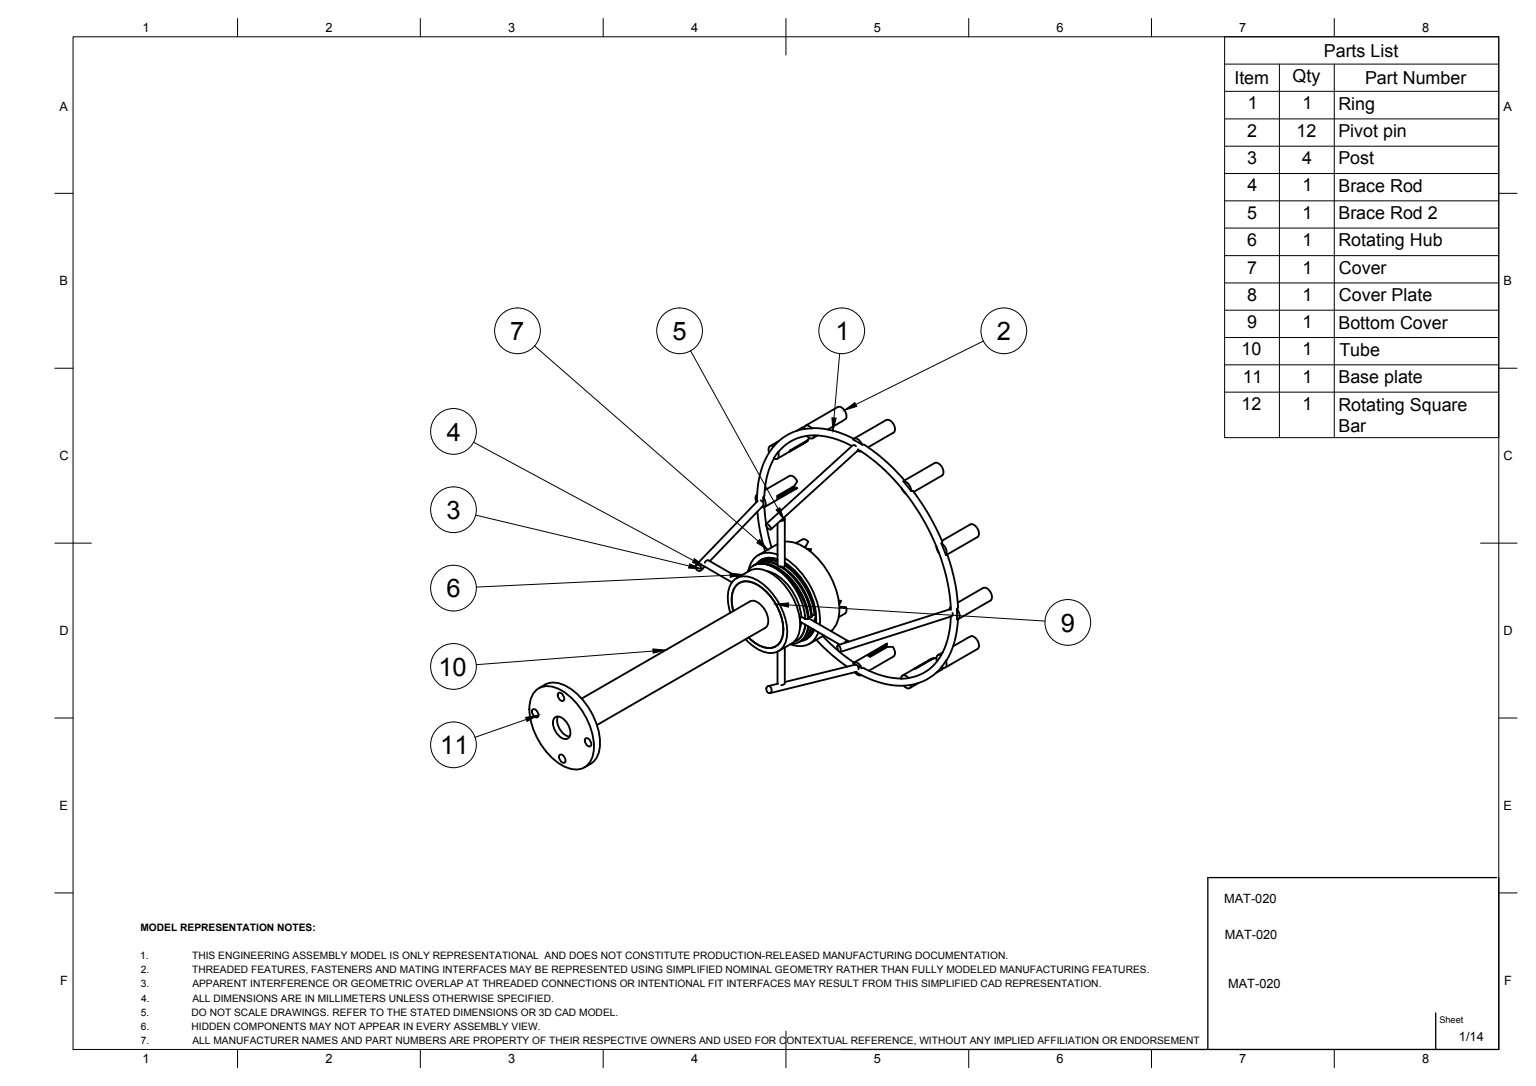
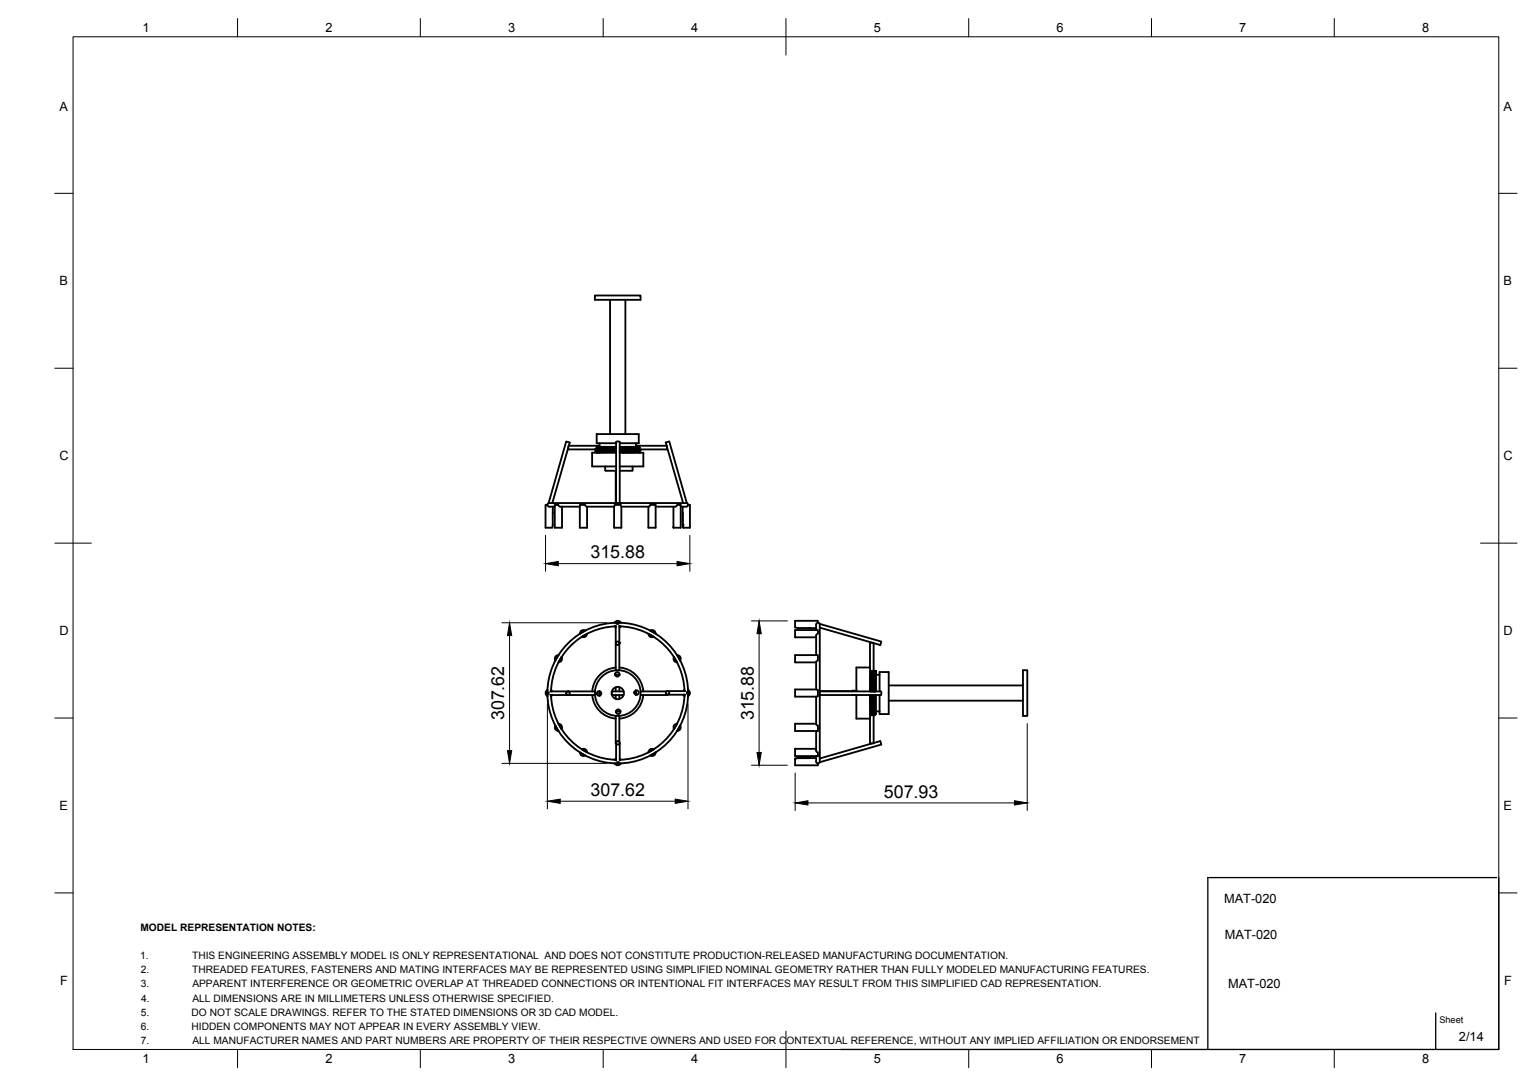
ISO-10303-21;
HEADER;
/* Generated by software containing ST-Developer
 * from STEP Tools, Inc. (www.steptools.com) 
 */

FILE_DESCRIPTION(
/* description */ ('STEP AP214'),
/* implementation_level */ '2;1');

FILE_NAME(
/* name */ 'MAT-020.step',
/* time_stamp */ '2026-11-14T06:20:50-08:00',
/* author */ (''),
/* organization */ (''),
/* preprocessor_version */ 'ST-DEVELOPER v20.2',
/* originating_system */ 'Autodesk Translation Framework v15.17.0.0',
/* authorisation */ '');

FILE_SCHEMA (('AUTOMOTIVE_DESIGN { 1 0 10303 214 3 1 1 }'));
ENDSEC;

DATA;
#10=MECHANICAL_DESIGN_GEOMETRIC_PRESENTATION_REPRESENTATION('',(#956,#957,
#958,#959,#960,#961,#962,#963,#964,#965,#966,#967),#20658);
#11=ITEM_DEFINED_TRANSFORMATION($,$,#3797,#4103);
#12=ITEM_DEFINED_TRANSFORMATION($,$,#4072,#4104);
#13=ITEM_DEFINED_TRANSFORMATION($,$,#4066,#4105);
#14=ITEM_DEFINED_TRANSFORMATION($,$,#3801,#4106);
#15=ITEM_DEFINED_TRANSFORMATION($,$,#3807,#4107);
#16=ITEM_DEFINED_TRANSFORMATION($,$,#3813,#4108);
#17=ITEM_DEFINED_TRANSFORMATION($,$,#3932,#4109);
#18=ITEM_DEFINED_TRANSFORMATION($,$,#3966,#4110);
#19=ITEM_DEFINED_TRANSFORMATION($,$,#3972,#4111);
#20=ITEM_DEFINED_TRANSFORMATION($,$,#3981,#4112);
#21=ITEM_DEFINED_TRANSFORMATION($,$,#3990,#4113);
#22=ITEM_DEFINED_TRANSFORMATION($,$,#4015,#4114);
#23=ITEM_DEFINED_TRANSFORMATION($,$,#4066,#4115);
#24=ITEM_DEFINED_TRANSFORMATION($,$,#4066,#4116);
#25=ITEM_DEFINED_TRANSFORMATION($,$,#4066,#4117);
#26=ITEM_DEFINED_TRANSFORMATION($,$,#4072,#4118);
#27=ITEM_DEFINED_TRANSFORMATION($,$,#4072,#4119);
#28=ITEM_DEFINED_TRANSFORMATION($,$,#4072,#4120);
#29=ITEM_DEFINED_TRANSFORMATION($,$,#4072,#4121);
#30=ITEM_DEFINED_TRANSFORMATION($,$,#4072,#4122);
#31=ITEM_DEFINED_TRANSFORMATION($,$,#4072,#4123);
#32=ITEM_DEFINED_TRANSFORMATION($,$,#4072,#4124);
#33=ITEM_DEFINED_TRANSFORMATION($,$,#4072,#4125);
#34=ITEM_DEFINED_TRANSFORMATION($,$,#4072,#4126);
#35=ITEM_DEFINED_TRANSFORMATION($,$,#4072,#4127);
#36=ITEM_DEFINED_TRANSFORMATION($,$,#4072,#4128);
#37=(
REPRESENTATION_RELATIONSHIP($,$,#20716,#20715)
REPRESENTATION_RELATIONSHIP_WITH_TRANSFORMATION(#11)
SHAPE_REPRESENTATION_RELATIONSHIP()
);
#38=(
REPRESENTATION_RELATIONSHIP($,$,#20727,#20715)
REPRESENTATION_RELATIONSHIP_WITH_TRANSFORMATION(#12)
SHAPE_REPRESENTATION_RELATIONSHIP()
);
#39=(
REPRESENTATION_RELATIONSHIP($,$,#20726,#20715)
REPRESENTATION_RELATIONSHIP_WITH_TRANSFORMATION(#13)
SHAPE_REPRESENTATION_RELATIONSHIP()
);
#40=(
REPRESENTATION_RELATIONSHIP($,$,#20717,#20715)
REPRESENTATION_RELATIONSHIP_WITH_TRANSFORMATION(#14)
SHAPE_REPRESENTATION_RELATIONSHIP()
);
#41=(
REPRESENTATION_RELATIONSHIP($,$,#20718,#20715)
REPRESENTATION_RELATIONSHIP_WITH_TRANSFORMATION(#15)
SHAPE_REPRESENTATION_RELATIONSHIP()
);
#42=(
REPRESENTATION_RELATIONSHIP($,$,#20719,#20715)
REPRESENTATION_RELATIONSHIP_WITH_TRANSFORMATION(#16)
SHAPE_REPRESENTATION_RELATIONSHIP()
);
#43=(
REPRESENTATION_RELATIONSHIP($,$,#20720,#20715)
REPRESENTATION_RELATIONSHIP_WITH_TRANSFORMATION(#17)
SHAPE_REPRESENTATION_RELATIONSHIP()
);
#44=(
REPRESENTATION_RELATIONSHIP($,$,#20721,#20715)
REPRESENTATION_RELATIONSHIP_WITH_TRANSFORMATION(#18)
SHAPE_REPRESENTATION_RELATIONSHIP()
);
#45=(
REPRESENTATION_RELATIONSHIP($,$,#20722,#20715)
REPRESENTATION_RELATIONSHIP_WITH_TRANSFORMATION(#19)
SHAPE_REPRESENTATION_RELATIONSHIP()
);
#46=(
REPRESENTATION_RELATIONSHIP($,$,#20723,#20715)
REPRESENTATION_RELATIONSHIP_WITH_TRANSFORMATION(#20)
SHAPE_REPRESENTATION_RELATIONSHIP()
);
#47=(
REPRESENTATION_RELATIONSHIP($,$,#20724,#20715)
REPRESENTATION_RELATIONSHIP_WITH_TRANSFORMATION(#21)
SHAPE_REPRESENTATION_RELATIONSHIP()
);
#48=(
REPRESENTATION_RELATIONSHIP($,$,#20725,#20715)
REPRESENTATION_RELATIONSHIP_WITH_TRANSFORMATION(#22)
SHAPE_REPRESENTATION_RELATIONSHIP()
);
#49=(
REPRESENTATION_RELATIONSHIP($,$,#20726,#20715)
REPRESENTATION_RELATIONSHIP_WITH_TRANSFORMATION(#23)
SHAPE_REPRESENTATION_RELATIONSHIP()
);
#50=(
REPRESENTATION_RELATIONSHIP($,$,#20726,#20715)
REPRESENTATION_RELATIONSHIP_WITH_TRANSFORMATION(#24)
SHAPE_REPRESENTATION_RELATIONSHIP()
);
#51=(
REPRESENTATION_RELATIONSHIP($,$,#20726,#20715)
REPRESENTATION_RELATIONSHIP_WITH_TRANSFORMATION(#25)
SHAPE_REPRESENTATION_RELATIONSHIP()
);
#52=(
REPRESENTATION_RELATIONSHIP($,$,#20727,#20715)
REPRESENTATION_RELATIONSHIP_WITH_TRANSFORMATION(#26)
SHAPE_REPRESENTATION_RELATIONSHIP()
);
#53=(
REPRESENTATION_RELATIONSHIP($,$,#20727,#20715)
REPRESENTATION_RELATIONSHIP_WITH_TRANSFORMATION(#27)
SHAPE_REPRESENTATION_RELATIONSHIP()
);
#54=(
REPRESENTATION_RELATIONSHIP($,$,#20727,#20715)
REPRESENTATION_RELATIONSHIP_WITH_TRANSFORMATION(#28)
SHAPE_REPRESENTATION_RELATIONSHIP()
);
#55=(
REPRESENTATION_RELATIONSHIP($,$,#20727,#20715)
REPRESENTATION_RELATIONSHIP_WITH_TRANSFORMATION(#29)
SHAPE_REPRESENTATION_RELATIONSHIP()
);
#56=(
REPRESENTATION_RELATIONSHIP($,$,#20727,#20715)
REPRESENTATION_RELATIONSHIP_WITH_TRANSFORMATION(#30)
SHAPE_REPRESENTATION_RELATIONSHIP()
);
#57=(
REPRESENTATION_RELATIONSHIP($,$,#20727,#20715)
REPRESENTATION_RELATIONSHIP_WITH_TRANSFORMATION(#31)
SHAPE_REPRESENTATION_RELATIONSHIP()
);
#58=(
REPRESENTATION_RELATIONSHIP($,$,#20727,#20715)
REPRESENTATION_RELATIONSHIP_WITH_TRANSFORMATION(#32)
SHAPE_REPRESENTATION_RELATIONSHIP()
);
#59=(
REPRESENTATION_RELATIONSHIP($,$,#20727,#20715)
REPRESENTATION_RELATIONSHIP_WITH_TRANSFORMATION(#33)
SHAPE_REPRESENTATION_RELATIONSHIP()
);
#60=(
REPRESENTATION_RELATIONSHIP($,$,#20727,#20715)
REPRESENTATION_RELATIONSHIP_WITH_TRANSFORMATION(#34)
SHAPE_REPRESENTATION_RELATIONSHIP()
);
#61=(
REPRESENTATION_RELATIONSHIP($,$,#20727,#20715)
REPRESENTATION_RELATIONSHIP_WITH_TRANSFORMATION(#35)
SHAPE_REPRESENTATION_RELATIONSHIP()
);
#62=(
REPRESENTATION_RELATIONSHIP($,$,#20727,#20715)
REPRESENTATION_RELATIONSHIP_WITH_TRANSFORMATION(#36)
SHAPE_REPRESENTATION_RELATIONSHIP()
);
#63=CONTEXT_DEPENDENT_SHAPE_REPRESENTATION(#37,#20689);
#64=CONTEXT_DEPENDENT_SHAPE_REPRESENTATION(#38,#20690);
#65=CONTEXT_DEPENDENT_SHAPE_REPRESENTATION(#39,#20691);
#66=CONTEXT_DEPENDENT_SHAPE_REPRESENTATION(#40,#20692);
#67=CONTEXT_DEPENDENT_SHAPE_REPRESENTATION(#41,#20693);
#68=CONTEXT_DEPENDENT_SHAPE_REPRESENTATION(#42,#20694);
#69=CONTEXT_DEPENDENT_SHAPE_REPRESENTATION(#43,#20695);
#70=CONTEXT_DEPENDENT_SHAPE_REPRESENTATION(#44,#20696);
#71=CONTEXT_DEPENDENT_SHAPE_REPRESENTATION(#45,#20697);
#72=CONTEXT_DEPENDENT_SHAPE_REPRESENTATION(#46,#20698);
#73=CONTEXT_DEPENDENT_SHAPE_REPRESENTATION(#47,#20699);
#74=CONTEXT_DEPENDENT_SHAPE_REPRESENTATION(#48,#20700);
#75=CONTEXT_DEPENDENT_SHAPE_REPRESENTATION(#49,#20701);
#76=CONTEXT_DEPENDENT_SHAPE_REPRESENTATION(#50,#20702);
#77=CONTEXT_DEPENDENT_SHAPE_REPRESENTATION(#51,#20703);
#78=CONTEXT_DEPENDENT_SHAPE_REPRESENTATION(#52,#20704);
#79=CONTEXT_DEPENDENT_SHAPE_REPRESENTATION(#53,#20705);
#80=CONTEXT_DEPENDENT_SHAPE_REPRESENTATION(#54,#20706);
#81=CONTEXT_DEPENDENT_SHAPE_REPRESENTATION(#55,#20707);
#82=CONTEXT_DEPENDENT_SHAPE_REPRESENTATION(#56,#20708);
#83=CONTEXT_DEPENDENT_SHAPE_REPRESENTATION(#57,#20709);
#84=CONTEXT_DEPENDENT_SHAPE_REPRESENTATION(#58,#20710);
#85=CONTEXT_DEPENDENT_SHAPE_REPRESENTATION(#59,#20711);
#86=CONTEXT_DEPENDENT_SHAPE_REPRESENTATION(#60,#20712);
#87=CONTEXT_DEPENDENT_SHAPE_REPRESENTATION(#61,#20713);
#88=CONTEXT_DEPENDENT_SHAPE_REPRESENTATION(#62,#20714);
#89=NEXT_ASSEMBLY_USAGE_OCCURRENCE('Ring:1','Ring:1','Ring:1',#20729,#20730,
'Ring:1');
#90=NEXT_ASSEMBLY_USAGE_OCCURRENCE('Pivot Pin:1','Pivot Pin:1',
'Pivot Pin:1',#20729,#20741,'Pivot Pin:1');
#91=NEXT_ASSEMBLY_USAGE_OCCURRENCE('Post:1','Post:1','Post:1',#20729,#20740,
'Post:1');
#92=NEXT_ASSEMBLY_USAGE_OCCURRENCE('Brace Rod:1','Brace Rod:1',
'Brace Rod:1',#20729,#20731,'Brace Rod:1');
#93=NEXT_ASSEMBLY_USAGE_OCCURRENCE('Brace Rod 2:1','Brace Rod 2:1',
'Brace Rod 2:1',#20729,#20732,'Brace Rod 2:1');
#94=NEXT_ASSEMBLY_USAGE_OCCURRENCE('Rotating Hub:1','Rotating Hub:1',
'Rotating Hub:1',#20729,#20733,'Rotating Hub:1');
#95=NEXT_ASSEMBLY_USAGE_OCCURRENCE('Cover:1','Cover:1','Cover:1',#20729,
#20734,'Cover:1');
#96=NEXT_ASSEMBLY_USAGE_OCCURRENCE('Cover Plate:1','Cover Plate:1',
'Cover Plate:1',#20729,#20735,'Cover Plate:1');
#97=NEXT_ASSEMBLY_USAGE_OCCURRENCE('Bottom Cover:1','Bottom Cover:1',
'Bottom Cover:1',#20729,#20736,'Bottom Cover:1');
#98=NEXT_ASSEMBLY_USAGE_OCCURRENCE('Tube:1','Tube:1','Tube:1',#20729,#20737,
'Tube:1');
#99=NEXT_ASSEMBLY_USAGE_OCCURRENCE('Base Plate:1','Base Plate:1',
'Base Plate:1',#20729,#20738,'Base Plate:1');
#100=NEXT_ASSEMBLY_USAGE_OCCURRENCE('Rotating Square Bar:1',
'Rotating Square Bar:1','Rotating Square Bar:1',#20729,#20739,
'Rotating Square Bar:1');
#101=NEXT_ASSEMBLY_USAGE_OCCURRENCE('Post:2','Post:2','Post:2',#20729,#20740,
'Post:2');
#102=NEXT_ASSEMBLY_USAGE_OCCURRENCE('Post:3','Post:3','Post:3',#20729,#20740,
'Post:3');
#103=NEXT_ASSEMBLY_USAGE_OCCURRENCE('Post:4','Post:4','Post:4',#20729,#20740,
'Post:4');
#104=NEXT_ASSEMBLY_USAGE_OCCURRENCE('Pivot Pin:2','Pivot Pin:2',
'Pivot Pin:2',#20729,#20741,'Pivot Pin:2');
#105=NEXT_ASSEMBLY_USAGE_OCCURRENCE('Pivot Pin:3','Pivot Pin:3',
'Pivot Pin:3',#20729,#20741,'Pivot Pin:3');
#106=NEXT_ASSEMBLY_USAGE_OCCURRENCE('Pivot Pin:4','Pivot Pin:4',
'Pivot Pin:4',#20729,#20741,'Pivot Pin:4');
#107=NEXT_ASSEMBLY_USAGE_OCCURRENCE('Pivot Pin:5','Pivot Pin:5',
'Pivot Pin:5',#20729,#20741,'Pivot Pin:5');
#108=NEXT_ASSEMBLY_USAGE_OCCURRENCE('Pivot Pin:6','Pivot Pin:6',
'Pivot Pin:6',#20729,#20741,'Pivot Pin:6');
#109=NEXT_ASSEMBLY_USAGE_OCCURRENCE('Pivot Pin:7','Pivot Pin:7',
'Pivot Pin:7',#20729,#20741,'Pivot Pin:7');
#110=NEXT_ASSEMBLY_USAGE_OCCURRENCE('Pivot Pin:8','Pivot Pin:8',
'Pivot Pin:8',#20729,#20741,'Pivot Pin:8');
#111=NEXT_ASSEMBLY_USAGE_OCCURRENCE('Pivot Pin:9','Pivot Pin:9',
'Pivot Pin:9',#20729,#20741,'Pivot Pin:9');
#112=NEXT_ASSEMBLY_USAGE_OCCURRENCE('Pivot Pin:10','Pivot Pin:10',
'Pivot Pin:10',#20729,#20741,'Pivot Pin:10');
#113=NEXT_ASSEMBLY_USAGE_OCCURRENCE('Pivot Pin:11','Pivot Pin:11',
'Pivot Pin:11',#20729,#20741,'Pivot Pin:11');
#114=NEXT_ASSEMBLY_USAGE_OCCURRENCE('Pivot Pin:12','Pivot Pin:12',
'Pivot Pin:12',#20729,#20741,'Pivot Pin:12');
#115=CONICAL_SURFACE('',#4073,6.35000000000001,0.785398163397456);
#116=SPHERICAL_SURFACE('',#4025,1.);
#117=SPHERICAL_SURFACE('',#4028,1.);
#118=SPHERICAL_SURFACE('',#4045,1.);
#119=SPHERICAL_SURFACE('',#4047,1.);
#120=SPHERICAL_SURFACE('',#4049,1.);
#121=SPHERICAL_SURFACE('',#4051,1.);
#122=SPHERICAL_SURFACE('',#4061,1.);
#123=SPHERICAL_SURFACE('',#4063,1.);
#124=FACE_BOUND('',#1300,.T.);
#125=FACE_BOUND('',#1302,.T.);
#126=FACE_BOUND('',#1314,.T.);
#127=FACE_BOUND('',#1332,.T.);
#128=FACE_BOUND('',#1334,.T.);
#129=FACE_BOUND('',#1338,.T.);
#130=FACE_BOUND('',#1340,.T.);
#131=FACE_BOUND('',#1342,.T.);
#132=FACE_BOUND('',#1349,.T.);
#133=FACE_BOUND('',#1351,.T.);
#134=FACE_BOUND('',#1355,.T.);
#135=FACE_BOUND('',#1357,.T.);
#136=FACE_BOUND('',#1366,.T.);
#137=FACE_BOUND('',#1367,.T.);
#138=FACE_BOUND('',#1368,.T.);
#139=FACE_BOUND('',#1369,.T.);
#140=FACE_BOUND('',#1370,.T.);
#141=FACE_BOUND('',#1372,.T.);
#142=FACE_BOUND('',#1373,.T.);
#143=FACE_BOUND('',#1374,.T.);
#144=FACE_BOUND('',#1375,.T.);
#145=FACE_BOUND('',#1376,.T.);
#146=FACE_BOUND('',#1378,.T.);
#147=ELLIPSE('',#3911,3.97203818895926,3.95968922073708);
#148=ELLIPSE('',#4079,13.8289418104825,6.34999999998296);
#149=ELLIPSE('',#4080,15.0727020037017,6.35000000001005);
#150=ELLIPSE('',#4086,17.286177263089,7.93749999997138);
#151=ELLIPSE('',#4088,18.840877504683,7.93750000004892);
#152=(
BOUNDED_SURFACE()
B_SPLINE_SURFACE(1,2,((#5540,#5541,#5542,#5543,#5544,#5545,#5546,#5547,
#5548,#5549,#5550,#5551,#5552,#5553,#5554,#5555,#5556,#5557,#5558,#5559,
#5560,#5561,#5562,#5563,#5564,#5565,#5566,#5567,#5568,#5569,#5570,#5571,
#5572,#5573,#5574,#5575,#5576,#5577,#5578,#5579,#5580,#5581,#5582,#5583,
#5584,#5585,#5586,#5587,#5588,#5589,#5590,#5591,#5592,#5593,#5594,#5595,
#5596,#5597,#5598,#5599,#5600,#5601,#5602,#5603,#5604,#5605,#5606,#5607,
#5608,#5609,#5610,#5611,#5612,#5613,#5614,#5615,#5616,#5617,#5618,#5619,
#5620,#5621,#5622,#5623,#5624,#5625,#5626,#5627,#5628,#5629,#5630,#5631,
#5632,#5633,#5634,#5635,#5636,#5637,#5638,#5639,#5640,#5641,#5642,#5643,
#5644,#5645,#5646,#5647,#5648,#5649,#5650,#5651,#5652,#5653,#5654,#5655,
#5656,#5657,#5658,#5659,#5660,#5661,#5662,#5663,#5664,#5665,#5666,#5667,
#5668,#5669,#5670,#5671,#5672,#5673,#5674,#5675,#5676,#5677,#5678,#5679,
#5680,#5681,#5682,#5683,#5684),(#5685,#5686,#5687,#5688,#5689,#5690,#5691,
#5692,#5693,#5694,#5695,#5696,#5697,#5698,#5699,#5700,#5701,#5702,#5703,
#5704,#5705,#5706,#5707,#5708,#5709,#5710,#5711,#5712,#5713,#5714,#5715,
#5716,#5717,#5718,#5719,#5720,#5721,#5722,#5723,#5724,#5725,#5726,#5727,
#5728,#5729,#5730,#5731,#5732,#5733,#5734,#5735,#5736,#5737,#5738,#5739,
#5740,#5741,#5742,#5743,#5744,#5745,#5746,#5747,#5748,#5749,#5750,#5751,
#5752,#5753,#5754,#5755,#5756,#5757,#5758,#5759,#5760,#5761,#5762,#5763,
#5764,#5765,#5766,#5767,#5768,#5769,#5770,#5771,#5772,#5773,#5774,#5775,
#5776,#5777,#5778,#5779,#5780,#5781,#5782,#5783,#5784,#5785,#5786,#5787,
#5788,#5789,#5790,#5791,#5792,#5793,#5794,#5795,#5796,#5797,#5798,#5799,
#5800,#5801,#5802,#5803,#5804,#5805,#5806,#5807,#5808,#5809,#5810,#5811,
#5812,#5813,#5814,#5815,#5816,#5817,#5818,#5819,#5820,#5821,#5822,#5823,
#5824,#5825,#5826,#5827,#5828,#5829)),.UNSPECIFIED.,.F.,.F.,.F.)
B_SPLINE_SURFACE_WITH_KNOTS((2,2),(3,2,2,2,2,2,2,2,2,2,2,2,2,2,2,2,2,2,
2,2,2,2,2,2,2,2,2,2,2,2,2,2,2,2,2,2,2,2,2,2,2,2,2,2,2,2,2,2,2,2,2,2,2,2,
2,2,2,2,2,2,2,2,2,2,2,2,2,2,2,2,2,2,3),(0.,1.),(0.,0.0138888888888889,0.0277777777777778,
0.0416666666666667,0.0555555555555556,0.0694444444444444,0.0833333333333333,
0.0972222222222222,0.111111111111111,0.125,0.138888888888889,0.152777777777778,
0.166666666666667,0.180555555555556,0.194444444444444,0.208333333333333,
0.222222222222222,0.236111111111111,0.25,0.263888888888889,0.277777777777778,
0.291666666666667,0.305555555555556,0.319444444444444,0.333333333333333,
0.347222222222222,0.361111111111111,0.375,0.388888888888889,0.402777777777778,
0.416666666666667,0.430555555555556,0.444444444444444,0.458333333333333,
0.472222222222222,0.486111111111111,0.5,0.513888888888889,0.527777777777778,
0.541666666666667,0.555555555555556,0.569444444444444,0.583333333333333,
0.597222222222222,0.611111111111111,0.625,0.638888888888889,0.652777777777778,
0.666666666666667,0.680555555555556,0.694444444444444,0.708333333333333,
0.722222222222222,0.736111111111111,0.75,0.763888888888889,0.777777777777778,
0.791666666666667,0.805555555555556,0.819444444444444,0.833333333333333,
0.847222222222222,0.861111111111111,0.875,0.888888888888889,0.902777777777778,
0.916666666666667,0.930555555555556,0.944444444444444,0.958333333333333,
0.972222222222222,0.986111111111111,1.),.UNSPECIFIED.)
GEOMETRIC_REPRESENTATION_ITEM()
RATIONAL_B_SPLINE_SURFACE(((1.,0.965925826289068,1.,0.965925826289068,1.,
0.965925826289068,1.,0.965925826289068,1.,0.965925826289068,1.,0.965925826289068,
1.,0.965925826289068,1.,0.965925826289068,1.,0.965925826289068,1.,0.965925826289068,
1.,0.965925826289068,1.,0.965925826289068,1.,0.965925826289068,1.,0.965925826289068,
1.,0.965925826289068,1.,0.965925826289068,1.,0.965925826289068,1.,0.965925826289068,
1.,0.965925826289068,1.,0.965925826289068,1.,0.965925826289068,1.,0.965925826289068,
1.,0.965925826289068,1.,0.965925826289068,1.,0.965925826289068,1.,0.965925826289068,
1.,0.965925826289068,1.,0.965925826289068,1.,0.965925826289068,1.,0.965925826289068,
1.,0.965925826289068,1.,0.965925826289068,1.,0.965925826289068,1.,0.965925826289068,
1.,0.965925826289068,1.,0.965925826289068,1.,0.965925826289068,1.,0.965925826289068,
1.,0.965925826289068,1.,0.965925826289068,1.,0.965925826289068,1.,0.965925826289068,
1.,0.965925826289068,1.,0.965925826289068,1.,0.965925826289068,1.,0.965925826289068,
1.,0.965925826289068,1.,0.965925826289068,1.,0.965925826289068,1.,0.965925826289068,
1.,0.965925826289068,1.,0.965925826289068,1.,0.965925826289068,1.,0.965925826289068,
1.,0.965925826289068,1.,0.965925826289068,1.,0.965925826289068,1.,0.965925826289068,
1.,0.965925826289068,1.,0.965925826289068,1.,0.965925826289068,1.,0.965925826289068,
1.,0.965925826289068,1.,0.965925826289068,1.,0.965925826289068,1.,0.965925826289068,
1.,0.965925826289068,1.,0.965925826289068,1.,0.965925826289068,1.,0.965925826289068,
1.,0.965925826289068,1.,0.965925826289068,1.),(1.,0.965925826289068,1.,
0.965925826289068,1.,0.965925826289068,1.,0.965925826289068,1.,0.965925826289068,
1.,0.965925826289068,1.,0.965925826289068,1.,0.965925826289068,1.,0.965925826289068,
1.,0.965925826289068,1.,0.965925826289068,1.,0.965925826289068,1.,0.965925826289068,
1.,0.965925826289068,1.,0.965925826289068,1.,0.965925826289068,1.,0.965925826289068,
1.,0.965925826289068,1.,0.965925826289068,1.,0.965925826289068,1.,0.965925826289068,
1.,0.965925826289068,1.,0.965925826289068,1.,0.965925826289068,1.,0.965925826289068,
1.,0.965925826289068,1.,0.965925826289068,1.,0.965925826289068,1.,0.965925826289068,
1.,0.965925826289068,1.,0.965925826289068,1.,0.965925826289068,1.,0.965925826289068,
1.,0.965925826289068,1.,0.965925826289068,1.,0.965925826289068,1.,0.965925826289068,
1.,0.965925826289068,1.,0.965925826289068,1.,0.965925826289068,1.,0.965925826289068,
1.,0.965925826289068,1.,0.965925826289068,1.,0.965925826289068,1.,0.965925826289068,
1.,0.965925826289068,1.,0.965925826289068,1.,0.965925826289068,1.,0.965925826289068,
1.,0.965925826289068,1.,0.965925826289068,1.,0.965925826289068,1.,0.965925826289068,
1.,0.965925826289068,1.,0.965925826289068,1.,0.965925826289068,1.,0.965925826289068,
1.,0.965925826289068,1.,0.965925826289068,1.,0.965925826289068,1.,0.965925826289068,
1.,0.965925826289068,1.,0.965925826289068,1.,0.965925826289068,1.,0.965925826289068,
1.,0.965925826289068,1.,0.965925826289068,1.,0.965925826289068,1.,0.965925826289068,
1.,0.965925826289068,1.,0.965925826289068,1.,0.965925826289068,1.)))
REPRESENTATION_ITEM('')
SURFACE()
);
#153=(
BOUNDED_SURFACE()
B_SPLINE_SURFACE(1,2,((#5847,#5848,#5849,#5850,#5851,#5852,#5853,#5854,
#5855,#5856,#5857,#5858,#5859,#5860,#5861,#5862,#5863,#5864,#5865,#5866,
#5867,#5868,#5869,#5870,#5871,#5872,#5873,#5874,#5875,#5876,#5877,#5878,
#5879,#5880,#5881,#5882,#5883,#5884,#5885,#5886,#5887,#5888,#5889,#5890,
#5891,#5892,#5893,#5894,#5895,#5896,#5897,#5898,#5899,#5900,#5901,#5902,
#5903,#5904,#5905,#5906,#5907,#5908,#5909,#5910,#5911,#5912,#5913,#5914,
#5915,#5916,#5917,#5918,#5919,#5920,#5921,#5922,#5923,#5924,#5925,#5926,
#5927,#5928,#5929,#5930,#5931,#5932,#5933,#5934,#5935,#5936,#5937,#5938,
#5939,#5940,#5941,#5942,#5943,#5944,#5945,#5946,#5947,#5948,#5949,#5950,
#5951,#5952,#5953,#5954,#5955,#5956,#5957,#5958,#5959,#5960,#5961,#5962,
#5963,#5964,#5965,#5966,#5967,#5968,#5969,#5970,#5971,#5972,#5973,#5974,
#5975,#5976,#5977,#5978,#5979,#5980,#5981,#5982,#5983,#5984,#5985,#5986,
#5987,#5988,#5989,#5990,#5991),(#5992,#5993,#5994,#5995,#5996,#5997,#5998,
#5999,#6000,#6001,#6002,#6003,#6004,#6005,#6006,#6007,#6008,#6009,#6010,
#6011,#6012,#6013,#6014,#6015,#6016,#6017,#6018,#6019,#6020,#6021,#6022,
#6023,#6024,#6025,#6026,#6027,#6028,#6029,#6030,#6031,#6032,#6033,#6034,
#6035,#6036,#6037,#6038,#6039,#6040,#6041,#6042,#6043,#6044,#6045,#6046,
#6047,#6048,#6049,#6050,#6051,#6052,#6053,#6054,#6055,#6056,#6057,#6058,
#6059,#6060,#6061,#6062,#6063,#6064,#6065,#6066,#6067,#6068,#6069,#6070,
#6071,#6072,#6073,#6074,#6075,#6076,#6077,#6078,#6079,#6080,#6081,#6082,
#6083,#6084,#6085,#6086,#6087,#6088,#6089,#6090,#6091,#6092,#6093,#6094,
#6095,#6096,#6097,#6098,#6099,#6100,#6101,#6102,#6103,#6104,#6105,#6106,
#6107,#6108,#6109,#6110,#6111,#6112,#6113,#6114,#6115,#6116,#6117,#6118,
#6119,#6120,#6121,#6122,#6123,#6124,#6125,#6126,#6127,#6128,#6129,#6130,
#6131,#6132,#6133,#6134,#6135,#6136)),.UNSPECIFIED.,.F.,.F.,.F.)
B_SPLINE_SURFACE_WITH_KNOTS((2,2),(3,2,2,2,2,2,2,2,2,2,2,2,2,2,2,2,2,2,
2,2,2,2,2,2,2,2,2,2,2,2,2,2,2,2,2,2,2,2,2,2,2,2,2,2,2,2,2,2,2,2,2,2,2,2,
2,2,2,2,2,2,2,2,2,2,2,2,2,2,2,2,2,2,3),(0.,1.),(0.,0.0138888888888889,0.0277777777777778,
0.0416666666666667,0.0555555555555556,0.0694444444444444,0.0833333333333333,
0.0972222222222222,0.111111111111111,0.125,0.138888888888889,0.152777777777778,
0.166666666666667,0.180555555555556,0.194444444444444,0.208333333333333,
0.222222222222222,0.236111111111111,0.25,0.263888888888889,0.277777777777778,
0.291666666666667,0.305555555555556,0.319444444444444,0.333333333333333,
0.347222222222222,0.361111111111111,0.375,0.388888888888889,0.402777777777778,
0.416666666666667,0.430555555555556,0.444444444444444,0.458333333333333,
0.472222222222222,0.486111111111111,0.5,0.513888888888889,0.527777777777778,
0.541666666666667,0.555555555555556,0.569444444444444,0.583333333333333,
0.597222222222222,0.611111111111111,0.625,0.638888888888889,0.652777777777778,
0.666666666666667,0.680555555555556,0.694444444444444,0.708333333333333,
0.722222222222222,0.736111111111111,0.75,0.763888888888889,0.777777777777778,
0.791666666666667,0.805555555555556,0.819444444444444,0.833333333333333,
0.847222222222222,0.861111111111111,0.875,0.888888888888889,0.902777777777778,
0.916666666666667,0.930555555555556,0.944444444444444,0.958333333333333,
0.972222222222222,0.986111111111111,1.),.UNSPECIFIED.)
GEOMETRIC_REPRESENTATION_ITEM()
RATIONAL_B_SPLINE_SURFACE(((1.,0.965925826289068,1.,0.965925826289068,1.,
0.965925826289068,1.,0.965925826289068,1.,0.965925826289068,1.,0.965925826289068,
1.,0.965925826289068,1.,0.965925826289068,1.,0.965925826289068,1.,0.965925826289068,
1.,0.965925826289068,1.,0.965925826289068,1.,0.965925826289068,1.,0.965925826289068,
1.,0.965925826289068,1.,0.965925826289068,1.,0.965925826289068,1.,0.965925826289068,
1.,0.965925826289068,1.,0.965925826289068,1.,0.965925826289068,1.,0.965925826289068,
1.,0.965925826289068,1.,0.965925826289068,1.,0.965925826289068,1.,0.965925826289068,
1.,0.965925826289068,1.,0.965925826289068,1.,0.965925826289068,1.,0.965925826289068,
1.,0.965925826289068,1.,0.965925826289068,1.,0.965925826289068,1.,0.965925826289068,
1.,0.965925826289068,1.,0.965925826289068,1.,0.965925826289068,1.,0.965925826289068,
1.,0.965925826289068,1.,0.965925826289068,1.,0.965925826289068,1.,0.965925826289068,
1.,0.965925826289068,1.,0.965925826289068,1.,0.965925826289068,1.,0.965925826289068,
1.,0.965925826289068,1.,0.965925826289068,1.,0.965925826289068,1.,0.965925826289068,
1.,0.965925826289068,1.,0.965925826289068,1.,0.965925826289068,1.,0.965925826289068,
1.,0.965925826289068,1.,0.965925826289068,1.,0.965925826289068,1.,0.965925826289068,
1.,0.965925826289068,1.,0.965925826289068,1.,0.965925826289068,1.,0.965925826289068,
1.,0.965925826289068,1.,0.965925826289068,1.,0.965925826289068,1.,0.965925826289068,
1.,0.965925826289068,1.,0.965925826289068,1.,0.965925826289068,1.,0.965925826289068,
1.,0.965925826289068,1.,0.965925826289068,1.),(1.,0.965925826289068,1.,
0.965925826289068,1.,0.965925826289068,1.,0.965925826289068,1.,0.965925826289068,
1.,0.965925826289068,1.,0.965925826289068,1.,0.965925826289068,1.,0.965925826289068,
1.,0.965925826289068,1.,0.965925826289068,1.,0.965925826289068,1.,0.965925826289068,
1.,0.965925826289068,1.,0.965925826289068,1.,0.965925826289068,1.,0.965925826289068,
1.,0.965925826289068,1.,0.965925826289068,1.,0.965925826289068,1.,0.965925826289068,
1.,0.965925826289068,1.,0.965925826289068,1.,0.965925826289068,1.,0.965925826289068,
1.,0.965925826289068,1.,0.965925826289068,1.,0.965925826289068,1.,0.965925826289068,
1.,0.965925826289068,1.,0.965925826289068,1.,0.965925826289068,1.,0.965925826289068,
1.,0.965925826289068,1.,0.965925826289068,1.,0.965925826289068,1.,0.965925826289068,
1.,0.965925826289068,1.,0.965925826289068,1.,0.965925826289068,1.,0.965925826289068,
1.,0.965925826289068,1.,0.965925826289068,1.,0.965925826289068,1.,0.965925826289068,
1.,0.965925826289068,1.,0.965925826289068,1.,0.965925826289068,1.,0.965925826289068,
1.,0.965925826289068,1.,0.965925826289068,1.,0.965925826289068,1.,0.965925826289068,
1.,0.965925826289068,1.,0.965925826289068,1.,0.965925826289068,1.,0.965925826289068,
1.,0.965925826289068,1.,0.965925826289068,1.,0.965925826289068,1.,0.965925826289068,
1.,0.965925826289068,1.,0.965925826289068,1.,0.965925826289068,1.,0.965925826289068,
1.,0.965925826289068,1.,0.965925826289068,1.,0.965925826289068,1.,0.965925826289068,
1.,0.965925826289068,1.,0.965925826289068,1.,0.965925826289068,1.)))
REPRESENTATION_ITEM('')
SURFACE()
);
#154=(
BOUNDED_SURFACE()
B_SPLINE_SURFACE(1,2,((#6162,#6163,#6164,#6165,#6166,#6167,#6168,#6169,
#6170,#6171,#6172,#6173,#6174,#6175,#6176,#6177,#6178,#6179,#6180,#6181,
#6182,#6183,#6184,#6185,#6186,#6187,#6188,#6189,#6190,#6191,#6192,#6193,
#6194,#6195,#6196,#6197,#6198,#6199,#6200,#6201,#6202,#6203,#6204,#6205,
#6206,#6207,#6208,#6209,#6210,#6211,#6212,#6213,#6214,#6215,#6216,#6217,
#6218,#6219,#6220,#6221,#6222,#6223,#6224,#6225,#6226,#6227,#6228,#6229,
#6230,#6231,#6232,#6233,#6234,#6235,#6236,#6237,#6238,#6239,#6240,#6241,
#6242,#6243,#6244,#6245,#6246,#6247,#6248,#6249,#6250,#6251,#6252,#6253,
#6254,#6255,#6256,#6257,#6258,#6259,#6260,#6261,#6262,#6263,#6264,#6265,
#6266,#6267,#6268,#6269,#6270,#6271,#6272,#6273,#6274,#6275,#6276,#6277,
#6278,#6279,#6280,#6281,#6282,#6283,#6284,#6285,#6286,#6287,#6288,#6289,
#6290,#6291,#6292,#6293,#6294,#6295,#6296,#6297,#6298,#6299,#6300,#6301,
#6302,#6303,#6304,#6305,#6306),(#6307,#6308,#6309,#6310,#6311,#6312,#6313,
#6314,#6315,#6316,#6317,#6318,#6319,#6320,#6321,#6322,#6323,#6324,#6325,
#6326,#6327,#6328,#6329,#6330,#6331,#6332,#6333,#6334,#6335,#6336,#6337,
#6338,#6339,#6340,#6341,#6342,#6343,#6344,#6345,#6346,#6347,#6348,#6349,
#6350,#6351,#6352,#6353,#6354,#6355,#6356,#6357,#6358,#6359,#6360,#6361,
#6362,#6363,#6364,#6365,#6366,#6367,#6368,#6369,#6370,#6371,#6372,#6373,
#6374,#6375,#6376,#6377,#6378,#6379,#6380,#6381,#6382,#6383,#6384,#6385,
#6386,#6387,#6388,#6389,#6390,#6391,#6392,#6393,#6394,#6395,#6396,#6397,
#6398,#6399,#6400,#6401,#6402,#6403,#6404,#6405,#6406,#6407,#6408,#6409,
#6410,#6411,#6412,#6413,#6414,#6415,#6416,#6417,#6418,#6419,#6420,#6421,
#6422,#6423,#6424,#6425,#6426,#6427,#6428,#6429,#6430,#6431,#6432,#6433,
#6434,#6435,#6436,#6437,#6438,#6439,#6440,#6441,#6442,#6443,#6444,#6445,
#6446,#6447,#6448,#6449,#6450,#6451)),.UNSPECIFIED.,.F.,.F.,.F.)
B_SPLINE_SURFACE_WITH_KNOTS((2,2),(3,2,2,2,2,2,2,2,2,2,2,2,2,2,2,2,2,2,
2,2,2,2,2,2,2,2,2,2,2,2,2,2,2,2,2,2,2,2,2,2,2,2,2,2,2,2,2,2,2,2,2,2,2,2,
2,2,2,2,2,2,2,2,2,2,2,2,2,2,2,2,2,2,3),(0.,1.),(0.,0.0138888888888889,0.0277777777777778,
0.0416666666666667,0.0555555555555556,0.0694444444444444,0.0833333333333333,
0.0972222222222222,0.111111111111111,0.125,0.138888888888889,0.152777777777778,
0.166666666666667,0.180555555555556,0.194444444444444,0.208333333333333,
0.222222222222222,0.236111111111111,0.25,0.263888888888889,0.277777777777778,
0.291666666666667,0.305555555555556,0.319444444444444,0.333333333333333,
0.347222222222222,0.361111111111111,0.375,0.388888888888889,0.402777777777778,
0.416666666666667,0.430555555555556,0.444444444444444,0.458333333333333,
0.472222222222222,0.486111111111111,0.5,0.513888888888889,0.527777777777778,
0.541666666666667,0.555555555555556,0.569444444444444,0.583333333333333,
0.597222222222222,0.611111111111111,0.625,0.638888888888889,0.652777777777778,
0.666666666666667,0.680555555555556,0.694444444444444,0.708333333333333,
0.722222222222222,0.736111111111111,0.75,0.763888888888889,0.777777777777778,
0.791666666666667,0.805555555555556,0.819444444444444,0.833333333333333,
0.847222222222222,0.861111111111111,0.875,0.888888888888889,0.902777777777778,
0.916666666666667,0.930555555555556,0.944444444444444,0.958333333333333,
0.972222222222222,0.986111111111111,1.),.UNSPECIFIED.)
GEOMETRIC_REPRESENTATION_ITEM()
RATIONAL_B_SPLINE_SURFACE(((1.,0.965925826289068,1.,0.965925826289068,1.,
0.965925826289068,1.,0.965925826289068,1.,0.965925826289068,1.,0.965925826289068,
1.,0.965925826289068,1.,0.965925826289068,1.,0.965925826289068,1.,0.965925826289068,
1.,0.965925826289068,1.,0.965925826289068,1.,0.965925826289068,1.,0.965925826289068,
1.,0.965925826289068,1.,0.965925826289068,1.,0.965925826289068,1.,0.965925826289068,
1.,0.965925826289068,1.,0.965925826289068,1.,0.965925826289068,1.,0.965925826289068,
1.,0.965925826289068,1.,0.965925826289068,1.,0.965925826289068,1.,0.965925826289068,
1.,0.965925826289068,1.,0.965925826289068,1.,0.965925826289068,1.,0.965925826289068,
1.,0.965925826289068,1.,0.965925826289068,1.,0.965925826289068,1.,0.965925826289068,
1.,0.965925826289068,1.,0.965925826289068,1.,0.965925826289068,1.,0.965925826289068,
1.,0.965925826289068,1.,0.965925826289068,1.,0.965925826289068,1.,0.965925826289068,
1.,0.965925826289068,1.,0.965925826289068,1.,0.965925826289068,1.,0.965925826289068,
1.,0.965925826289068,1.,0.965925826289068,1.,0.965925826289068,1.,0.965925826289068,
1.,0.965925826289068,1.,0.965925826289068,1.,0.965925826289068,1.,0.965925826289068,
1.,0.965925826289068,1.,0.965925826289068,1.,0.965925826289068,1.,0.965925826289068,
1.,0.965925826289068,1.,0.965925826289068,1.,0.965925826289068,1.,0.965925826289068,
1.,0.965925826289068,1.,0.965925826289068,1.,0.965925826289068,1.,0.965925826289068,
1.,0.965925826289068,1.,0.965925826289068,1.,0.965925826289068,1.,0.965925826289068,
1.,0.965925826289068,1.,0.965925826289068,1.),(1.,0.965925826289068,1.,
0.965925826289068,1.,0.965925826289068,1.,0.965925826289068,1.,0.965925826289068,
1.,0.965925826289068,1.,0.965925826289068,1.,0.965925826289068,1.,0.965925826289068,
1.,0.965925826289068,1.,0.965925826289068,1.,0.965925826289068,1.,0.965925826289068,
1.,0.965925826289068,1.,0.965925826289068,1.,0.965925826289068,1.,0.965925826289068,
1.,0.965925826289068,1.,0.965925826289068,1.,0.965925826289068,1.,0.965925826289068,
1.,0.965925826289068,1.,0.965925826289068,1.,0.965925826289068,1.,0.965925826289068,
1.,0.965925826289068,1.,0.965925826289068,1.,0.965925826289068,1.,0.965925826289068,
1.,0.965925826289068,1.,0.965925826289068,1.,0.965925826289068,1.,0.965925826289068,
1.,0.965925826289068,1.,0.965925826289068,1.,0.965925826289068,1.,0.965925826289068,
1.,0.965925826289068,1.,0.965925826289068,1.,0.965925826289068,1.,0.965925826289068,
1.,0.965925826289068,1.,0.965925826289068,1.,0.965925826289068,1.,0.965925826289068,
1.,0.965925826289068,1.,0.965925826289068,1.,0.965925826289068,1.,0.965925826289068,
1.,0.965925826289068,1.,0.965925826289068,1.,0.965925826289068,1.,0.965925826289068,
1.,0.965925826289068,1.,0.965925826289068,1.,0.965925826289068,1.,0.965925826289068,
1.,0.965925826289068,1.,0.965925826289068,1.,0.965925826289068,1.,0.965925826289068,
1.,0.965925826289068,1.,0.965925826289068,1.,0.965925826289068,1.,0.965925826289068,
1.,0.965925826289068,1.,0.965925826289068,1.,0.965925826289068,1.,0.965925826289068,
1.,0.965925826289068,1.,0.965925826289068,1.,0.965925826289068,1.)))
REPRESENTATION_ITEM('')
SURFACE()
);
#155=(
BOUNDED_SURFACE()
B_SPLINE_SURFACE(1,2,((#6469,#6470,#6471,#6472,#6473,#6474,#6475,#6476,
#6477,#6478,#6479,#6480,#6481,#6482,#6483,#6484,#6485,#6486,#6487,#6488,
#6489,#6490,#6491,#6492,#6493,#6494,#6495,#6496,#6497,#6498,#6499,#6500,
#6501,#6502,#6503,#6504,#6505,#6506,#6507,#6508,#6509,#6510,#6511,#6512,
#6513,#6514,#6515,#6516,#6517,#6518,#6519,#6520,#6521,#6522,#6523,#6524,
#6525,#6526,#6527,#6528,#6529,#6530,#6531,#6532,#6533,#6534,#6535,#6536,
#6537,#6538,#6539,#6540,#6541,#6542,#6543,#6544,#6545,#6546,#6547,#6548,
#6549,#6550,#6551,#6552,#6553,#6554,#6555,#6556,#6557,#6558,#6559,#6560,
#6561,#6562,#6563,#6564,#6565,#6566,#6567,#6568,#6569,#6570,#6571,#6572,
#6573,#6574,#6575,#6576,#6577,#6578,#6579,#6580,#6581,#6582,#6583,#6584,
#6585,#6586,#6587,#6588,#6589,#6590,#6591,#6592,#6593,#6594,#6595,#6596,
#6597,#6598,#6599,#6600,#6601,#6602,#6603,#6604,#6605,#6606,#6607,#6608,
#6609,#6610,#6611,#6612,#6613),(#6614,#6615,#6616,#6617,#6618,#6619,#6620,
#6621,#6622,#6623,#6624,#6625,#6626,#6627,#6628,#6629,#6630,#6631,#6632,
#6633,#6634,#6635,#6636,#6637,#6638,#6639,#6640,#6641,#6642,#6643,#6644,
#6645,#6646,#6647,#6648,#6649,#6650,#6651,#6652,#6653,#6654,#6655,#6656,
#6657,#6658,#6659,#6660,#6661,#6662,#6663,#6664,#6665,#6666,#6667,#6668,
#6669,#6670,#6671,#6672,#6673,#6674,#6675,#6676,#6677,#6678,#6679,#6680,
#6681,#6682,#6683,#6684,#6685,#6686,#6687,#6688,#6689,#6690,#6691,#6692,
#6693,#6694,#6695,#6696,#6697,#6698,#6699,#6700,#6701,#6702,#6703,#6704,
#6705,#6706,#6707,#6708,#6709,#6710,#6711,#6712,#6713,#6714,#6715,#6716,
#6717,#6718,#6719,#6720,#6721,#6722,#6723,#6724,#6725,#6726,#6727,#6728,
#6729,#6730,#6731,#6732,#6733,#6734,#6735,#6736,#6737,#6738,#6739,#6740,
#6741,#6742,#6743,#6744,#6745,#6746,#6747,#6748,#6749,#6750,#6751,#6752,
#6753,#6754,#6755,#6756,#6757,#6758)),.UNSPECIFIED.,.F.,.F.,.F.)
B_SPLINE_SURFACE_WITH_KNOTS((2,2),(3,2,2,2,2,2,2,2,2,2,2,2,2,2,2,2,2,2,
2,2,2,2,2,2,2,2,2,2,2,2,2,2,2,2,2,2,2,2,2,2,2,2,2,2,2,2,2,2,2,2,2,2,2,2,
2,2,2,2,2,2,2,2,2,2,2,2,2,2,2,2,2,2,3),(0.,1.),(0.,0.0138888888888889,0.0277777777777778,
0.0416666666666667,0.0555555555555556,0.0694444444444444,0.0833333333333333,
0.0972222222222222,0.111111111111111,0.125,0.138888888888889,0.152777777777778,
0.166666666666667,0.180555555555556,0.194444444444444,0.208333333333333,
0.222222222222222,0.236111111111111,0.25,0.263888888888889,0.277777777777778,
0.291666666666667,0.305555555555556,0.319444444444444,0.333333333333333,
0.347222222222222,0.361111111111111,0.375,0.388888888888889,0.402777777777778,
0.416666666666667,0.430555555555556,0.444444444444444,0.458333333333333,
0.472222222222222,0.486111111111111,0.5,0.513888888888889,0.527777777777778,
0.541666666666667,0.555555555555556,0.569444444444444,0.583333333333333,
0.597222222222222,0.611111111111111,0.625,0.638888888888889,0.652777777777778,
0.666666666666667,0.680555555555556,0.694444444444444,0.708333333333333,
0.722222222222222,0.736111111111111,0.75,0.763888888888889,0.777777777777778,
0.791666666666667,0.805555555555556,0.819444444444444,0.833333333333333,
0.847222222222222,0.861111111111111,0.875,0.888888888888889,0.902777777777778,
0.916666666666667,0.930555555555556,0.944444444444444,0.958333333333333,
0.972222222222222,0.986111111111111,1.),.UNSPECIFIED.)
GEOMETRIC_REPRESENTATION_ITEM()
RATIONAL_B_SPLINE_SURFACE(((1.,0.965925826289068,1.,0.965925826289068,1.,
0.965925826289068,1.,0.965925826289068,1.,0.965925826289068,1.,0.965925826289068,
1.,0.965925826289068,1.,0.965925826289068,1.,0.965925826289068,1.,0.965925826289068,
1.,0.965925826289068,1.,0.965925826289068,1.,0.965925826289068,1.,0.965925826289068,
1.,0.965925826289068,1.,0.965925826289068,1.,0.965925826289068,1.,0.965925826289068,
1.,0.965925826289068,1.,0.965925826289068,1.,0.965925826289068,1.,0.965925826289068,
1.,0.965925826289068,1.,0.965925826289068,1.,0.965925826289068,1.,0.965925826289068,
1.,0.965925826289068,1.,0.965925826289068,1.,0.965925826289068,1.,0.965925826289068,
1.,0.965925826289068,1.,0.965925826289068,1.,0.965925826289068,1.,0.965925826289068,
1.,0.965925826289068,1.,0.965925826289068,1.,0.965925826289068,1.,0.965925826289068,
1.,0.965925826289068,1.,0.965925826289068,1.,0.965925826289068,1.,0.965925826289068,
1.,0.965925826289068,1.,0.965925826289068,1.,0.965925826289068,1.,0.965925826289068,
1.,0.965925826289068,1.,0.965925826289068,1.,0.965925826289068,1.,0.965925826289068,
1.,0.965925826289068,1.,0.965925826289068,1.,0.965925826289068,1.,0.965925826289068,
1.,0.965925826289068,1.,0.965925826289068,1.,0.965925826289068,1.,0.965925826289068,
1.,0.965925826289068,1.,0.965925826289068,1.,0.965925826289068,1.,0.965925826289068,
1.,0.965925826289068,1.,0.965925826289068,1.,0.965925826289068,1.,0.965925826289068,
1.,0.965925826289068,1.,0.965925826289068,1.,0.965925826289068,1.,0.965925826289068,
1.,0.965925826289068,1.,0.965925826289068,1.),(1.,0.965925826289068,1.,
0.965925826289068,1.,0.965925826289068,1.,0.965925826289068,1.,0.965925826289068,
1.,0.965925826289068,1.,0.965925826289068,1.,0.965925826289068,1.,0.965925826289068,
1.,0.965925826289068,1.,0.965925826289068,1.,0.965925826289068,1.,0.965925826289068,
1.,0.965925826289068,1.,0.965925826289068,1.,0.965925826289068,1.,0.965925826289068,
1.,0.965925826289068,1.,0.965925826289068,1.,0.965925826289068,1.,0.965925826289068,
1.,0.965925826289068,1.,0.965925826289068,1.,0.965925826289068,1.,0.965925826289068,
1.,0.965925826289068,1.,0.965925826289068,1.,0.965925826289068,1.,0.965925826289068,
1.,0.965925826289068,1.,0.965925826289068,1.,0.965925826289068,1.,0.965925826289068,
1.,0.965925826289068,1.,0.965925826289068,1.,0.965925826289068,1.,0.965925826289068,
1.,0.965925826289068,1.,0.965925826289068,1.,0.965925826289068,1.,0.965925826289068,
1.,0.965925826289068,1.,0.965925826289068,1.,0.965925826289068,1.,0.965925826289068,
1.,0.965925826289068,1.,0.965925826289068,1.,0.965925826289068,1.,0.965925826289068,
1.,0.965925826289068,1.,0.965925826289068,1.,0.965925826289068,1.,0.965925826289068,
1.,0.965925826289068,1.,0.965925826289068,1.,0.965925826289068,1.,0.965925826289068,
1.,0.965925826289068,1.,0.965925826289068,1.,0.965925826289068,1.,0.965925826289068,
1.,0.965925826289068,1.,0.965925826289068,1.,0.965925826289068,1.,0.965925826289068,
1.,0.965925826289068,1.,0.965925826289068,1.,0.965925826289068,1.,0.965925826289068,
1.,0.965925826289068,1.,0.965925826289068,1.,0.965925826289068,1.)))
REPRESENTATION_ITEM('')
SURFACE()
);
#156=(
BOUNDED_SURFACE()
B_SPLINE_SURFACE(1,2,((#6784,#6785,#6786,#6787,#6788,#6789,#6790,#6791,
#6792,#6793,#6794,#6795,#6796,#6797,#6798,#6799,#6800,#6801,#6802,#6803,
#6804,#6805,#6806,#6807,#6808,#6809,#6810,#6811,#6812,#6813,#6814,#6815,
#6816,#6817,#6818,#6819,#6820,#6821,#6822,#6823,#6824,#6825,#6826,#6827,
#6828,#6829,#6830,#6831,#6832,#6833,#6834,#6835,#6836,#6837,#6838,#6839,
#6840,#6841,#6842,#6843,#6844,#6845,#6846,#6847,#6848,#6849,#6850,#6851,
#6852,#6853,#6854,#6855,#6856,#6857,#6858,#6859,#6860,#6861,#6862,#6863,
#6864,#6865,#6866,#6867,#6868,#6869,#6870,#6871,#6872,#6873,#6874,#6875,
#6876,#6877,#6878,#6879,#6880,#6881,#6882,#6883,#6884,#6885,#6886,#6887,
#6888,#6889,#6890,#6891,#6892,#6893,#6894,#6895,#6896,#6897,#6898,#6899,
#6900,#6901,#6902,#6903,#6904,#6905,#6906,#6907,#6908,#6909,#6910,#6911,
#6912,#6913,#6914,#6915,#6916,#6917,#6918,#6919,#6920,#6921,#6922,#6923,
#6924,#6925,#6926,#6927,#6928),(#6929,#6930,#6931,#6932,#6933,#6934,#6935,
#6936,#6937,#6938,#6939,#6940,#6941,#6942,#6943,#6944,#6945,#6946,#6947,
#6948,#6949,#6950,#6951,#6952,#6953,#6954,#6955,#6956,#6957,#6958,#6959,
#6960,#6961,#6962,#6963,#6964,#6965,#6966,#6967,#6968,#6969,#6970,#6971,
#6972,#6973,#6974,#6975,#6976,#6977,#6978,#6979,#6980,#6981,#6982,#6983,
#6984,#6985,#6986,#6987,#6988,#6989,#6990,#6991,#6992,#6993,#6994,#6995,
#6996,#6997,#6998,#6999,#7000,#7001,#7002,#7003,#7004,#7005,#7006,#7007,
#7008,#7009,#7010,#7011,#7012,#7013,#7014,#7015,#7016,#7017,#7018,#7019,
#7020,#7021,#7022,#7023,#7024,#7025,#7026,#7027,#7028,#7029,#7030,#7031,
#7032,#7033,#7034,#7035,#7036,#7037,#7038,#7039,#7040,#7041,#7042,#7043,
#7044,#7045,#7046,#7047,#7048,#7049,#7050,#7051,#7052,#7053,#7054,#7055,
#7056,#7057,#7058,#7059,#7060,#7061,#7062,#7063,#7064,#7065,#7066,#7067,
#7068,#7069,#7070,#7071,#7072,#7073)),.UNSPECIFIED.,.F.,.F.,.F.)
B_SPLINE_SURFACE_WITH_KNOTS((2,2),(3,2,2,2,2,2,2,2,2,2,2,2,2,2,2,2,2,2,
2,2,2,2,2,2,2,2,2,2,2,2,2,2,2,2,2,2,2,2,2,2,2,2,2,2,2,2,2,2,2,2,2,2,2,2,
2,2,2,2,2,2,2,2,2,2,2,2,2,2,2,2,2,2,3),(0.,1.),(0.,0.0138888888888889,0.0277777777777778,
0.0416666666666667,0.0555555555555556,0.0694444444444444,0.0833333333333333,
0.0972222222222222,0.111111111111111,0.125,0.138888888888889,0.152777777777778,
0.166666666666667,0.180555555555556,0.194444444444444,0.208333333333333,
0.222222222222222,0.236111111111111,0.25,0.263888888888889,0.277777777777778,
0.291666666666667,0.305555555555556,0.319444444444444,0.333333333333333,
0.347222222222222,0.361111111111111,0.375,0.388888888888889,0.402777777777778,
0.416666666666667,0.430555555555556,0.444444444444444,0.458333333333333,
0.472222222222222,0.486111111111111,0.5,0.513888888888889,0.527777777777778,
0.541666666666667,0.555555555555556,0.569444444444444,0.583333333333333,
0.597222222222222,0.611111111111111,0.625,0.638888888888889,0.652777777777778,
0.666666666666667,0.680555555555556,0.694444444444444,0.708333333333333,
0.722222222222222,0.736111111111111,0.75,0.763888888888889,0.777777777777778,
0.791666666666667,0.805555555555556,0.819444444444444,0.833333333333333,
0.847222222222222,0.861111111111111,0.875,0.888888888888889,0.902777777777778,
0.916666666666667,0.930555555555556,0.944444444444444,0.958333333333333,
0.972222222222222,0.986111111111111,1.),.UNSPECIFIED.)
GEOMETRIC_REPRESENTATION_ITEM()
RATIONAL_B_SPLINE_SURFACE(((1.,0.965925826289068,1.,0.965925826289068,1.,
0.965925826289068,1.,0.965925826289068,1.,0.965925826289068,1.,0.965925826289068,
1.,0.965925826289068,1.,0.965925826289068,1.,0.965925826289068,1.,0.965925826289068,
1.,0.965925826289068,1.,0.965925826289068,1.,0.965925826289068,1.,0.965925826289068,
1.,0.965925826289068,1.,0.965925826289068,1.,0.965925826289068,1.,0.965925826289068,
1.,0.965925826289068,1.,0.965925826289068,1.,0.965925826289068,1.,0.965925826289068,
1.,0.965925826289068,1.,0.965925826289068,1.,0.965925826289068,1.,0.965925826289068,
1.,0.965925826289068,1.,0.965925826289068,1.,0.965925826289068,1.,0.965925826289068,
1.,0.965925826289068,1.,0.965925826289068,1.,0.965925826289068,1.,0.965925826289068,
1.,0.965925826289068,1.,0.965925826289068,1.,0.965925826289068,1.,0.965925826289068,
1.,0.965925826289068,1.,0.965925826289068,1.,0.965925826289068,1.,0.965925826289068,
1.,0.965925826289068,1.,0.965925826289068,1.,0.965925826289068,1.,0.965925826289068,
1.,0.965925826289068,1.,0.965925826289068,1.,0.965925826289068,1.,0.965925826289068,
1.,0.965925826289068,1.,0.965925826289068,1.,0.965925826289068,1.,0.965925826289068,
1.,0.965925826289068,1.,0.965925826289068,1.,0.965925826289068,1.,0.965925826289068,
1.,0.965925826289068,1.,0.965925826289068,1.,0.965925826289068,1.,0.965925826289068,
1.,0.965925826289068,1.,0.965925826289068,1.,0.965925826289068,1.,0.965925826289068,
1.,0.965925826289068,1.,0.965925826289068,1.,0.965925826289068,1.,0.965925826289068,
1.,0.965925826289068,1.,0.965925826289068,1.),(1.,0.965925826289068,1.,
0.965925826289068,1.,0.965925826289068,1.,0.965925826289068,1.,0.965925826289068,
1.,0.965925826289068,1.,0.965925826289068,1.,0.965925826289068,1.,0.965925826289068,
1.,0.965925826289068,1.,0.965925826289068,1.,0.965925826289068,1.,0.965925826289068,
1.,0.965925826289068,1.,0.965925826289068,1.,0.965925826289068,1.,0.965925826289068,
1.,0.965925826289068,1.,0.965925826289068,1.,0.965925826289068,1.,0.965925826289068,
1.,0.965925826289068,1.,0.965925826289068,1.,0.965925826289068,1.,0.965925826289068,
1.,0.965925826289068,1.,0.965925826289068,1.,0.965925826289068,1.,0.965925826289068,
1.,0.965925826289068,1.,0.965925826289068,1.,0.965925826289068,1.,0.965925826289068,
1.,0.965925826289068,1.,0.965925826289068,1.,0.965925826289068,1.,0.965925826289068,
1.,0.965925826289068,1.,0.965925826289068,1.,0.965925826289068,1.,0.965925826289068,
1.,0.965925826289068,1.,0.965925826289068,1.,0.965925826289068,1.,0.965925826289068,
1.,0.965925826289068,1.,0.965925826289068,1.,0.965925826289068,1.,0.965925826289068,
1.,0.965925826289068,1.,0.965925826289068,1.,0.965925826289068,1.,0.965925826289068,
1.,0.965925826289068,1.,0.965925826289068,1.,0.965925826289068,1.,0.965925826289068,
1.,0.965925826289068,1.,0.965925826289068,1.,0.965925826289068,1.,0.965925826289068,
1.,0.965925826289068,1.,0.965925826289068,1.,0.965925826289068,1.,0.965925826289068,
1.,0.965925826289068,1.,0.965925826289068,1.,0.965925826289068,1.,0.965925826289068,
1.,0.965925826289068,1.,0.965925826289068,1.,0.965925826289068,1.)))
REPRESENTATION_ITEM('')
SURFACE()
);
#157=(
BOUNDED_SURFACE()
B_SPLINE_SURFACE(1,2,((#7091,#7092,#7093,#7094,#7095,#7096,#7097,#7098,
#7099,#7100,#7101,#7102,#7103,#7104,#7105,#7106,#7107,#7108,#7109,#7110,
#7111,#7112,#7113,#7114,#7115,#7116,#7117,#7118,#7119,#7120,#7121,#7122,
#7123,#7124,#7125,#7126,#7127,#7128,#7129,#7130,#7131,#7132,#7133,#7134,
#7135,#7136,#7137,#7138,#7139,#7140,#7141,#7142,#7143,#7144,#7145,#7146,
#7147,#7148,#7149,#7150,#7151,#7152,#7153,#7154,#7155,#7156,#7157,#7158,
#7159,#7160,#7161,#7162,#7163,#7164,#7165,#7166,#7167,#7168,#7169,#7170,
#7171,#7172,#7173,#7174,#7175,#7176,#7177,#7178,#7179,#7180,#7181,#7182,
#7183,#7184,#7185,#7186,#7187,#7188,#7189,#7190,#7191,#7192,#7193,#7194,
#7195,#7196,#7197,#7198,#7199,#7200,#7201,#7202,#7203,#7204,#7205,#7206,
#7207,#7208,#7209,#7210,#7211,#7212,#7213,#7214,#7215,#7216,#7217,#7218,
#7219,#7220,#7221,#7222,#7223,#7224,#7225,#7226,#7227,#7228,#7229,#7230,
#7231,#7232,#7233,#7234,#7235),(#7236,#7237,#7238,#7239,#7240,#7241,#7242,
#7243,#7244,#7245,#7246,#7247,#7248,#7249,#7250,#7251,#7252,#7253,#7254,
#7255,#7256,#7257,#7258,#7259,#7260,#7261,#7262,#7263,#7264,#7265,#7266,
#7267,#7268,#7269,#7270,#7271,#7272,#7273,#7274,#7275,#7276,#7277,#7278,
#7279,#7280,#7281,#7282,#7283,#7284,#7285,#7286,#7287,#7288,#7289,#7290,
#7291,#7292,#7293,#7294,#7295,#7296,#7297,#7298,#7299,#7300,#7301,#7302,
#7303,#7304,#7305,#7306,#7307,#7308,#7309,#7310,#7311,#7312,#7313,#7314,
#7315,#7316,#7317,#7318,#7319,#7320,#7321,#7322,#7323,#7324,#7325,#7326,
#7327,#7328,#7329,#7330,#7331,#7332,#7333,#7334,#7335,#7336,#7337,#7338,
#7339,#7340,#7341,#7342,#7343,#7344,#7345,#7346,#7347,#7348,#7349,#7350,
#7351,#7352,#7353,#7354,#7355,#7356,#7357,#7358,#7359,#7360,#7361,#7362,
#7363,#7364,#7365,#7366,#7367,#7368,#7369,#7370,#7371,#7372,#7373,#7374,
#7375,#7376,#7377,#7378,#7379,#7380)),.UNSPECIFIED.,.F.,.F.,.F.)
B_SPLINE_SURFACE_WITH_KNOTS((2,2),(3,2,2,2,2,2,2,2,2,2,2,2,2,2,2,2,2,2,
2,2,2,2,2,2,2,2,2,2,2,2,2,2,2,2,2,2,2,2,2,2,2,2,2,2,2,2,2,2,2,2,2,2,2,2,
2,2,2,2,2,2,2,2,2,2,2,2,2,2,2,2,2,2,3),(0.,1.),(0.,0.0138888888888889,0.0277777777777778,
0.0416666666666667,0.0555555555555556,0.0694444444444444,0.0833333333333333,
0.0972222222222222,0.111111111111111,0.125,0.138888888888889,0.152777777777778,
0.166666666666667,0.180555555555556,0.194444444444444,0.208333333333333,
0.222222222222222,0.236111111111111,0.25,0.263888888888889,0.277777777777778,
0.291666666666667,0.305555555555556,0.319444444444444,0.333333333333333,
0.347222222222222,0.361111111111111,0.375,0.388888888888889,0.402777777777778,
0.416666666666667,0.430555555555556,0.444444444444444,0.458333333333333,
0.472222222222222,0.486111111111111,0.5,0.513888888888889,0.527777777777778,
0.541666666666667,0.555555555555556,0.569444444444444,0.583333333333333,
0.597222222222222,0.611111111111111,0.625,0.638888888888889,0.652777777777778,
0.666666666666667,0.680555555555556,0.694444444444444,0.708333333333333,
0.722222222222222,0.736111111111111,0.75,0.763888888888889,0.777777777777778,
0.791666666666667,0.805555555555556,0.819444444444444,0.833333333333333,
0.847222222222222,0.861111111111111,0.875,0.888888888888889,0.902777777777778,
0.916666666666667,0.930555555555556,0.944444444444444,0.958333333333333,
0.972222222222222,0.986111111111111,1.),.UNSPECIFIED.)
GEOMETRIC_REPRESENTATION_ITEM()
RATIONAL_B_SPLINE_SURFACE(((1.,0.965925826289068,1.,0.965925826289068,1.,
0.965925826289068,1.,0.965925826289068,1.,0.965925826289068,1.,0.965925826289068,
1.,0.965925826289068,1.,0.965925826289068,1.,0.965925826289068,1.,0.965925826289068,
1.,0.965925826289068,1.,0.965925826289068,1.,0.965925826289068,1.,0.965925826289068,
1.,0.965925826289068,1.,0.965925826289068,1.,0.965925826289068,1.,0.965925826289068,
1.,0.965925826289068,1.,0.965925826289068,1.,0.965925826289068,1.,0.965925826289068,
1.,0.965925826289068,1.,0.965925826289068,1.,0.965925826289068,1.,0.965925826289068,
1.,0.965925826289068,1.,0.965925826289068,1.,0.965925826289068,1.,0.965925826289068,
1.,0.965925826289068,1.,0.965925826289068,1.,0.965925826289068,1.,0.965925826289068,
1.,0.965925826289068,1.,0.965925826289068,1.,0.965925826289068,1.,0.965925826289068,
1.,0.965925826289068,1.,0.965925826289068,1.,0.965925826289068,1.,0.965925826289068,
1.,0.965925826289068,1.,0.965925826289068,1.,0.965925826289068,1.,0.965925826289068,
1.,0.965925826289068,1.,0.965925826289068,1.,0.965925826289068,1.,0.965925826289068,
1.,0.965925826289068,1.,0.965925826289068,1.,0.965925826289068,1.,0.965925826289068,
1.,0.965925826289068,1.,0.965925826289068,1.,0.965925826289068,1.,0.965925826289068,
1.,0.965925826289068,1.,0.965925826289068,1.,0.965925826289068,1.,0.965925826289068,
1.,0.965925826289068,1.,0.965925826289068,1.,0.965925826289068,1.,0.965925826289068,
1.,0.965925826289068,1.,0.965925826289068,1.,0.965925826289068,1.,0.965925826289068,
1.,0.965925826289068,1.,0.965925826289068,1.),(1.,0.965925826289068,1.,
0.965925826289068,1.,0.965925826289068,1.,0.965925826289068,1.,0.965925826289068,
1.,0.965925826289068,1.,0.965925826289068,1.,0.965925826289068,1.,0.965925826289068,
1.,0.965925826289068,1.,0.965925826289068,1.,0.965925826289068,1.,0.965925826289068,
1.,0.965925826289068,1.,0.965925826289068,1.,0.965925826289068,1.,0.965925826289068,
1.,0.965925826289068,1.,0.965925826289068,1.,0.965925826289068,1.,0.965925826289068,
1.,0.965925826289068,1.,0.965925826289068,1.,0.965925826289068,1.,0.965925826289068,
1.,0.965925826289068,1.,0.965925826289068,1.,0.965925826289068,1.,0.965925826289068,
1.,0.965925826289068,1.,0.965925826289068,1.,0.965925826289068,1.,0.965925826289068,
1.,0.965925826289068,1.,0.965925826289068,1.,0.965925826289068,1.,0.965925826289068,
1.,0.965925826289068,1.,0.965925826289068,1.,0.965925826289068,1.,0.965925826289068,
1.,0.965925826289068,1.,0.965925826289068,1.,0.965925826289068,1.,0.965925826289068,
1.,0.965925826289068,1.,0.965925826289068,1.,0.965925826289068,1.,0.965925826289068,
1.,0.965925826289068,1.,0.965925826289068,1.,0.965925826289068,1.,0.965925826289068,
1.,0.965925826289068,1.,0.965925826289068,1.,0.965925826289068,1.,0.965925826289068,
1.,0.965925826289068,1.,0.965925826289068,1.,0.965925826289068,1.,0.965925826289068,
1.,0.965925826289068,1.,0.965925826289068,1.,0.965925826289068,1.,0.965925826289068,
1.,0.965925826289068,1.,0.965925826289068,1.,0.965925826289068,1.,0.965925826289068,
1.,0.965925826289068,1.,0.965925826289068,1.,0.965925826289068,1.)))
REPRESENTATION_ITEM('')
SURFACE()
);
#158=(
BOUNDED_SURFACE()
B_SPLINE_SURFACE(1,2,((#7406,#7407,#7408,#7409,#7410,#7411,#7412,#7413,
#7414,#7415,#7416,#7417,#7418,#7419,#7420,#7421,#7422,#7423,#7424,#7425,
#7426,#7427,#7428,#7429,#7430,#7431,#7432,#7433,#7434,#7435,#7436,#7437,
#7438,#7439,#7440,#7441,#7442,#7443,#7444,#7445,#7446,#7447,#7448,#7449,
#7450,#7451,#7452,#7453,#7454,#7455,#7456,#7457,#7458,#7459,#7460,#7461,
#7462,#7463,#7464,#7465,#7466,#7467,#7468,#7469,#7470,#7471,#7472,#7473,
#7474,#7475,#7476,#7477,#7478,#7479,#7480,#7481,#7482,#7483,#7484,#7485,
#7486,#7487,#7488,#7489,#7490,#7491,#7492,#7493,#7494,#7495,#7496,#7497,
#7498,#7499,#7500,#7501,#7502,#7503,#7504,#7505,#7506,#7507,#7508,#7509,
#7510,#7511,#7512,#7513,#7514,#7515,#7516,#7517,#7518,#7519,#7520,#7521,
#7522,#7523,#7524,#7525,#7526,#7527,#7528,#7529,#7530,#7531,#7532,#7533,
#7534,#7535,#7536,#7537,#7538,#7539,#7540,#7541,#7542,#7543,#7544,#7545,
#7546,#7547,#7548,#7549,#7550),(#7551,#7552,#7553,#7554,#7555,#7556,#7557,
#7558,#7559,#7560,#7561,#7562,#7563,#7564,#7565,#7566,#7567,#7568,#7569,
#7570,#7571,#7572,#7573,#7574,#7575,#7576,#7577,#7578,#7579,#7580,#7581,
#7582,#7583,#7584,#7585,#7586,#7587,#7588,#7589,#7590,#7591,#7592,#7593,
#7594,#7595,#7596,#7597,#7598,#7599,#7600,#7601,#7602,#7603,#7604,#7605,
#7606,#7607,#7608,#7609,#7610,#7611,#7612,#7613,#7614,#7615,#7616,#7617,
#7618,#7619,#7620,#7621,#7622,#7623,#7624,#7625,#7626,#7627,#7628,#7629,
#7630,#7631,#7632,#7633,#7634,#7635,#7636,#7637,#7638,#7639,#7640,#7641,
#7642,#7643,#7644,#7645,#7646,#7647,#7648,#7649,#7650,#7651,#7652,#7653,
#7654,#7655,#7656,#7657,#7658,#7659,#7660,#7661,#7662,#7663,#7664,#7665,
#7666,#7667,#7668,#7669,#7670,#7671,#7672,#7673,#7674,#7675,#7676,#7677,
#7678,#7679,#7680,#7681,#7682,#7683,#7684,#7685,#7686,#7687,#7688,#7689,
#7690,#7691,#7692,#7693,#7694,#7695)),.UNSPECIFIED.,.F.,.F.,.F.)
B_SPLINE_SURFACE_WITH_KNOTS((2,2),(3,2,2,2,2,2,2,2,2,2,2,2,2,2,2,2,2,2,
2,2,2,2,2,2,2,2,2,2,2,2,2,2,2,2,2,2,2,2,2,2,2,2,2,2,2,2,2,2,2,2,2,2,2,2,
2,2,2,2,2,2,2,2,2,2,2,2,2,2,2,2,2,2,3),(0.,1.),(0.,0.0138888888888889,0.0277777777777778,
0.0416666666666667,0.0555555555555556,0.0694444444444444,0.0833333333333333,
0.0972222222222222,0.111111111111111,0.125,0.138888888888889,0.152777777777778,
0.166666666666667,0.180555555555556,0.194444444444444,0.208333333333333,
0.222222222222222,0.236111111111111,0.25,0.263888888888889,0.277777777777778,
0.291666666666667,0.305555555555556,0.319444444444444,0.333333333333333,
0.347222222222222,0.361111111111111,0.375,0.388888888888889,0.402777777777778,
0.416666666666667,0.430555555555556,0.444444444444444,0.458333333333333,
0.472222222222222,0.486111111111111,0.5,0.513888888888889,0.527777777777778,
0.541666666666667,0.555555555555556,0.569444444444444,0.583333333333333,
0.597222222222222,0.611111111111111,0.625,0.638888888888889,0.652777777777778,
0.666666666666667,0.680555555555556,0.694444444444444,0.708333333333333,
0.722222222222222,0.736111111111111,0.75,0.763888888888889,0.777777777777778,
0.791666666666667,0.805555555555556,0.819444444444444,0.833333333333333,
0.847222222222222,0.861111111111111,0.875,0.888888888888889,0.902777777777778,
0.916666666666667,0.930555555555556,0.944444444444444,0.958333333333333,
0.972222222222222,0.986111111111111,1.),.UNSPECIFIED.)
GEOMETRIC_REPRESENTATION_ITEM()
RATIONAL_B_SPLINE_SURFACE(((1.,0.965925826289068,1.,0.965925826289068,1.,
0.965925826289068,1.,0.965925826289068,1.,0.965925826289068,1.,0.965925826289068,
1.,0.965925826289068,1.,0.965925826289068,1.,0.965925826289068,1.,0.965925826289068,
1.,0.965925826289068,1.,0.965925826289068,1.,0.965925826289068,1.,0.965925826289068,
1.,0.965925826289068,1.,0.965925826289068,1.,0.965925826289068,1.,0.965925826289068,
1.,0.965925826289068,1.,0.965925826289068,1.,0.965925826289068,1.,0.965925826289068,
1.,0.965925826289068,1.,0.965925826289068,1.,0.965925826289068,1.,0.965925826289068,
1.,0.965925826289068,1.,0.965925826289068,1.,0.965925826289068,1.,0.965925826289068,
1.,0.965925826289068,1.,0.965925826289068,1.,0.965925826289068,1.,0.965925826289068,
1.,0.965925826289068,1.,0.965925826289068,1.,0.965925826289068,1.,0.965925826289068,
1.,0.965925826289068,1.,0.965925826289068,1.,0.965925826289068,1.,0.965925826289068,
1.,0.965925826289068,1.,0.965925826289068,1.,0.965925826289068,1.,0.965925826289068,
1.,0.965925826289068,1.,0.965925826289068,1.,0.965925826289068,1.,0.965925826289068,
1.,0.965925826289068,1.,0.965925826289068,1.,0.965925826289068,1.,0.965925826289068,
1.,0.965925826289068,1.,0.965925826289068,1.,0.965925826289068,1.,0.965925826289068,
1.,0.965925826289068,1.,0.965925826289068,1.,0.965925826289068,1.,0.965925826289068,
1.,0.965925826289068,1.,0.965925826289068,1.,0.965925826289068,1.,0.965925826289068,
1.,0.965925826289068,1.,0.965925826289068,1.,0.965925826289068,1.,0.965925826289068,
1.,0.965925826289068,1.,0.965925826289068,1.),(1.,0.965925826289068,1.,
0.965925826289068,1.,0.965925826289068,1.,0.965925826289068,1.,0.965925826289068,
1.,0.965925826289068,1.,0.965925826289068,1.,0.965925826289068,1.,0.965925826289068,
1.,0.965925826289068,1.,0.965925826289068,1.,0.965925826289068,1.,0.965925826289068,
1.,0.965925826289068,1.,0.965925826289068,1.,0.965925826289068,1.,0.965925826289068,
1.,0.965925826289068,1.,0.965925826289068,1.,0.965925826289068,1.,0.965925826289068,
1.,0.965925826289068,1.,0.965925826289068,1.,0.965925826289068,1.,0.965925826289068,
1.,0.965925826289068,1.,0.965925826289068,1.,0.965925826289068,1.,0.965925826289068,
1.,0.965925826289068,1.,0.965925826289068,1.,0.965925826289068,1.,0.965925826289068,
1.,0.965925826289068,1.,0.965925826289068,1.,0.965925826289068,1.,0.965925826289068,
1.,0.965925826289068,1.,0.965925826289068,1.,0.965925826289068,1.,0.965925826289068,
1.,0.965925826289068,1.,0.965925826289068,1.,0.965925826289068,1.,0.965925826289068,
1.,0.965925826289068,1.,0.965925826289068,1.,0.965925826289068,1.,0.965925826289068,
1.,0.965925826289068,1.,0.965925826289068,1.,0.965925826289068,1.,0.965925826289068,
1.,0.965925826289068,1.,0.965925826289068,1.,0.965925826289068,1.,0.965925826289068,
1.,0.965925826289068,1.,0.965925826289068,1.,0.965925826289068,1.,0.965925826289068,
1.,0.965925826289068,1.,0.965925826289068,1.,0.965925826289068,1.,0.965925826289068,
1.,0.965925826289068,1.,0.965925826289068,1.,0.965925826289068,1.,0.965925826289068,
1.,0.965925826289068,1.,0.965925826289068,1.,0.965925826289068,1.)))
REPRESENTATION_ITEM('')
SURFACE()
);
#159=(
BOUNDED_SURFACE()
B_SPLINE_SURFACE(1,2,((#7713,#7714,#7715,#7716,#7717,#7718,#7719,#7720,
#7721,#7722,#7723,#7724,#7725,#7726,#7727,#7728,#7729,#7730,#7731,#7732,
#7733,#7734,#7735,#7736,#7737,#7738,#7739,#7740,#7741,#7742,#7743,#7744,
#7745,#7746,#7747,#7748,#7749,#7750,#7751,#7752,#7753,#7754,#7755,#7756,
#7757,#7758,#7759,#7760,#7761,#7762,#7763,#7764,#7765,#7766,#7767,#7768,
#7769,#7770,#7771,#7772,#7773,#7774,#7775,#7776,#7777,#7778,#7779,#7780,
#7781,#7782,#7783,#7784,#7785,#7786,#7787,#7788,#7789,#7790,#7791,#7792,
#7793,#7794,#7795,#7796,#7797,#7798,#7799,#7800,#7801,#7802,#7803,#7804,
#7805,#7806,#7807,#7808,#7809,#7810,#7811,#7812,#7813,#7814,#7815,#7816,
#7817,#7818,#7819,#7820,#7821,#7822,#7823,#7824,#7825,#7826,#7827,#7828,
#7829,#7830,#7831,#7832,#7833,#7834,#7835,#7836,#7837,#7838,#7839,#7840,
#7841,#7842,#7843,#7844,#7845,#7846,#7847,#7848,#7849,#7850,#7851,#7852,
#7853,#7854,#7855,#7856,#7857),(#7858,#7859,#7860,#7861,#7862,#7863,#7864,
#7865,#7866,#7867,#7868,#7869,#7870,#7871,#7872,#7873,#7874,#7875,#7876,
#7877,#7878,#7879,#7880,#7881,#7882,#7883,#7884,#7885,#7886,#7887,#7888,
#7889,#7890,#7891,#7892,#7893,#7894,#7895,#7896,#7897,#7898,#7899,#7900,
#7901,#7902,#7903,#7904,#7905,#7906,#7907,#7908,#7909,#7910,#7911,#7912,
#7913,#7914,#7915,#7916,#7917,#7918,#7919,#7920,#7921,#7922,#7923,#7924,
#7925,#7926,#7927,#7928,#7929,#7930,#7931,#7932,#7933,#7934,#7935,#7936,
#7937,#7938,#7939,#7940,#7941,#7942,#7943,#7944,#7945,#7946,#7947,#7948,
#7949,#7950,#7951,#7952,#7953,#7954,#7955,#7956,#7957,#7958,#7959,#7960,
#7961,#7962,#7963,#7964,#7965,#7966,#7967,#7968,#7969,#7970,#7971,#7972,
#7973,#7974,#7975,#7976,#7977,#7978,#7979,#7980,#7981,#7982,#7983,#7984,
#7985,#7986,#7987,#7988,#7989,#7990,#7991,#7992,#7993,#7994,#7995,#7996,
#7997,#7998,#7999,#8000,#8001,#8002)),.UNSPECIFIED.,.F.,.F.,.F.)
B_SPLINE_SURFACE_WITH_KNOTS((2,2),(3,2,2,2,2,2,2,2,2,2,2,2,2,2,2,2,2,2,
2,2,2,2,2,2,2,2,2,2,2,2,2,2,2,2,2,2,2,2,2,2,2,2,2,2,2,2,2,2,2,2,2,2,2,2,
2,2,2,2,2,2,2,2,2,2,2,2,2,2,2,2,2,2,3),(0.,1.),(0.,0.0138888888888889,0.0277777777777778,
0.0416666666666667,0.0555555555555556,0.0694444444444444,0.0833333333333333,
0.0972222222222222,0.111111111111111,0.125,0.138888888888889,0.152777777777778,
0.166666666666667,0.180555555555556,0.194444444444444,0.208333333333333,
0.222222222222222,0.236111111111111,0.25,0.263888888888889,0.277777777777778,
0.291666666666667,0.305555555555556,0.319444444444444,0.333333333333333,
0.347222222222222,0.361111111111111,0.375,0.388888888888889,0.402777777777778,
0.416666666666667,0.430555555555556,0.444444444444444,0.458333333333333,
0.472222222222222,0.486111111111111,0.5,0.513888888888889,0.527777777777778,
0.541666666666667,0.555555555555556,0.569444444444444,0.583333333333333,
0.597222222222222,0.611111111111111,0.625,0.638888888888889,0.652777777777778,
0.666666666666667,0.680555555555556,0.694444444444444,0.708333333333333,
0.722222222222222,0.736111111111111,0.75,0.763888888888889,0.777777777777778,
0.791666666666667,0.805555555555556,0.819444444444444,0.833333333333333,
0.847222222222222,0.861111111111111,0.875,0.888888888888889,0.902777777777778,
0.916666666666667,0.930555555555556,0.944444444444444,0.958333333333333,
0.972222222222222,0.986111111111111,1.),.UNSPECIFIED.)
GEOMETRIC_REPRESENTATION_ITEM()
RATIONAL_B_SPLINE_SURFACE(((1.,0.965925826289068,1.,0.965925826289068,1.,
0.965925826289068,1.,0.965925826289068,1.,0.965925826289068,1.,0.965925826289068,
1.,0.965925826289068,1.,0.965925826289068,1.,0.965925826289068,1.,0.965925826289068,
1.,0.965925826289068,1.,0.965925826289068,1.,0.965925826289068,1.,0.965925826289068,
1.,0.965925826289068,1.,0.965925826289068,1.,0.965925826289068,1.,0.965925826289068,
1.,0.965925826289068,1.,0.965925826289068,1.,0.965925826289068,1.,0.965925826289068,
1.,0.965925826289068,1.,0.965925826289068,1.,0.965925826289068,1.,0.965925826289068,
1.,0.965925826289068,1.,0.965925826289068,1.,0.965925826289068,1.,0.965925826289068,
1.,0.965925826289068,1.,0.965925826289068,1.,0.965925826289068,1.,0.965925826289068,
1.,0.965925826289068,1.,0.965925826289068,1.,0.965925826289068,1.,0.965925826289068,
1.,0.965925826289068,1.,0.965925826289068,1.,0.965925826289068,1.,0.965925826289068,
1.,0.965925826289068,1.,0.965925826289068,1.,0.965925826289068,1.,0.965925826289068,
1.,0.965925826289068,1.,0.965925826289068,1.,0.965925826289068,1.,0.965925826289068,
1.,0.965925826289068,1.,0.965925826289068,1.,0.965925826289068,1.,0.965925826289068,
1.,0.965925826289068,1.,0.965925826289068,1.,0.965925826289068,1.,0.965925826289068,
1.,0.965925826289068,1.,0.965925826289068,1.,0.965925826289068,1.,0.965925826289068,
1.,0.965925826289068,1.,0.965925826289068,1.,0.965925826289068,1.,0.965925826289068,
1.,0.965925826289068,1.,0.965925826289068,1.,0.965925826289068,1.,0.965925826289068,
1.,0.965925826289068,1.,0.965925826289068,1.),(1.,0.965925826289068,1.,
0.965925826289068,1.,0.965925826289068,1.,0.965925826289068,1.,0.965925826289068,
1.,0.965925826289068,1.,0.965925826289068,1.,0.965925826289068,1.,0.965925826289068,
1.,0.965925826289068,1.,0.965925826289068,1.,0.965925826289068,1.,0.965925826289068,
1.,0.965925826289068,1.,0.965925826289068,1.,0.965925826289068,1.,0.965925826289068,
1.,0.965925826289068,1.,0.965925826289068,1.,0.965925826289068,1.,0.965925826289068,
1.,0.965925826289068,1.,0.965925826289068,1.,0.965925826289068,1.,0.965925826289068,
1.,0.965925826289068,1.,0.965925826289068,1.,0.965925826289068,1.,0.965925826289068,
1.,0.965925826289068,1.,0.965925826289068,1.,0.965925826289068,1.,0.965925826289068,
1.,0.965925826289068,1.,0.965925826289068,1.,0.965925826289068,1.,0.965925826289068,
1.,0.965925826289068,1.,0.965925826289068,1.,0.965925826289068,1.,0.965925826289068,
1.,0.965925826289068,1.,0.965925826289068,1.,0.965925826289068,1.,0.965925826289068,
1.,0.965925826289068,1.,0.965925826289068,1.,0.965925826289068,1.,0.965925826289068,
1.,0.965925826289068,1.,0.965925826289068,1.,0.965925826289068,1.,0.965925826289068,
1.,0.965925826289068,1.,0.965925826289068,1.,0.965925826289068,1.,0.965925826289068,
1.,0.965925826289068,1.,0.965925826289068,1.,0.965925826289068,1.,0.965925826289068,
1.,0.965925826289068,1.,0.965925826289068,1.,0.965925826289068,1.,0.965925826289068,
1.,0.965925826289068,1.,0.965925826289068,1.,0.965925826289068,1.,0.965925826289068,
1.,0.965925826289068,1.,0.965925826289068,1.,0.965925826289068,1.)))
REPRESENTATION_ITEM('')
SURFACE()
);
#160=(
BOUNDED_SURFACE()
B_SPLINE_SURFACE(1,2,((#8031,#8032,#8033,#8034,#8035,#8036,#8037,#8038,
#8039,#8040,#8041,#8042,#8043,#8044,#8045,#8046,#8047,#8048,#8049,#8050,
#8051,#8052,#8053,#8054,#8055,#8056,#8057,#8058,#8059,#8060,#8061,#8062,
#8063,#8064,#8065,#8066,#8067,#8068,#8069,#8070,#8071,#8072,#8073,#8074,
#8075,#8076,#8077,#8078,#8079,#8080,#8081,#8082,#8083,#8084,#8085,#8086,
#8087,#8088,#8089,#8090,#8091,#8092,#8093,#8094,#8095,#8096,#8097,#8098,
#8099,#8100,#8101,#8102,#8103,#8104,#8105,#8106,#8107,#8108,#8109,#8110,
#8111,#8112,#8113,#8114,#8115,#8116,#8117,#8118,#8119,#8120,#8121,#8122,
#8123,#8124,#8125,#8126,#8127,#8128,#8129,#8130,#8131,#8132,#8133,#8134,
#8135,#8136,#8137,#8138,#8139,#8140,#8141,#8142,#8143,#8144,#8145,#8146,
#8147,#8148,#8149,#8150,#8151,#8152,#8153,#8154,#8155,#8156,#8157,#8158,
#8159,#8160,#8161,#8162,#8163,#8164,#8165,#8166,#8167,#8168,#8169,#8170,
#8171,#8172,#8173,#8174,#8175),(#8176,#8177,#8178,#8179,#8180,#8181,#8182,
#8183,#8184,#8185,#8186,#8187,#8188,#8189,#8190,#8191,#8192,#8193,#8194,
#8195,#8196,#8197,#8198,#8199,#8200,#8201,#8202,#8203,#8204,#8205,#8206,
#8207,#8208,#8209,#8210,#8211,#8212,#8213,#8214,#8215,#8216,#8217,#8218,
#8219,#8220,#8221,#8222,#8223,#8224,#8225,#8226,#8227,#8228,#8229,#8230,
#8231,#8232,#8233,#8234,#8235,#8236,#8237,#8238,#8239,#8240,#8241,#8242,
#8243,#8244,#8245,#8246,#8247,#8248,#8249,#8250,#8251,#8252,#8253,#8254,
#8255,#8256,#8257,#8258,#8259,#8260,#8261,#8262,#8263,#8264,#8265,#8266,
#8267,#8268,#8269,#8270,#8271,#8272,#8273,#8274,#8275,#8276,#8277,#8278,
#8279,#8280,#8281,#8282,#8283,#8284,#8285,#8286,#8287,#8288,#8289,#8290,
#8291,#8292,#8293,#8294,#8295,#8296,#8297,#8298,#8299,#8300,#8301,#8302,
#8303,#8304,#8305,#8306,#8307,#8308,#8309,#8310,#8311,#8312,#8313,#8314,
#8315,#8316,#8317,#8318,#8319,#8320)),.UNSPECIFIED.,.F.,.F.,.F.)
B_SPLINE_SURFACE_WITH_KNOTS((2,2),(3,2,2,2,2,2,2,2,2,2,2,2,2,2,2,2,2,2,
2,2,2,2,2,2,2,2,2,2,2,2,2,2,2,2,2,2,2,2,2,2,2,2,2,2,2,2,2,2,2,2,2,2,2,2,
2,2,2,2,2,2,2,2,2,2,2,2,2,2,2,2,2,2,3),(0.,1.),(0.,0.0138888888888889,0.0277777777777778,
0.0416666666666667,0.0555555555555556,0.0694444444444444,0.0833333333333333,
0.0972222222222222,0.111111111111111,0.125,0.138888888888889,0.152777777777778,
0.166666666666667,0.180555555555556,0.194444444444444,0.208333333333333,
0.222222222222222,0.236111111111111,0.25,0.263888888888889,0.277777777777778,
0.291666666666667,0.305555555555556,0.319444444444444,0.333333333333333,
0.347222222222222,0.361111111111111,0.375,0.388888888888889,0.402777777777778,
0.416666666666667,0.430555555555556,0.444444444444444,0.458333333333333,
0.472222222222222,0.486111111111111,0.5,0.513888888888889,0.527777777777778,
0.541666666666667,0.555555555555556,0.569444444444444,0.583333333333333,
0.597222222222222,0.611111111111111,0.625,0.638888888888889,0.652777777777778,
0.666666666666667,0.680555555555556,0.694444444444444,0.708333333333333,
0.722222222222222,0.736111111111111,0.75,0.763888888888889,0.777777777777778,
0.791666666666667,0.805555555555556,0.819444444444444,0.833333333333333,
0.847222222222222,0.861111111111111,0.875,0.888888888888889,0.902777777777778,
0.916666666666667,0.930555555555556,0.944444444444444,0.958333333333333,
0.972222222222222,0.986111111111111,1.),.UNSPECIFIED.)
GEOMETRIC_REPRESENTATION_ITEM()
RATIONAL_B_SPLINE_SURFACE(((1.,0.965925826289068,1.,0.965925826289068,1.,
0.965925826289068,1.,0.965925826289068,1.,0.965925826289068,1.,0.965925826289068,
1.,0.965925826289068,1.,0.965925826289068,1.,0.965925826289068,1.,0.965925826289068,
1.,0.965925826289068,1.,0.965925826289068,1.,0.965925826289068,1.,0.965925826289068,
1.,0.965925826289068,1.,0.965925826289068,1.,0.965925826289068,1.,0.965925826289068,
1.,0.965925826289068,1.,0.965925826289068,1.,0.965925826289068,1.,0.965925826289068,
1.,0.965925826289068,1.,0.965925826289068,1.,0.965925826289068,1.,0.965925826289068,
1.,0.965925826289068,1.,0.965925826289068,1.,0.965925826289068,1.,0.965925826289068,
1.,0.965925826289068,1.,0.965925826289068,1.,0.965925826289068,1.,0.965925826289068,
1.,0.965925826289068,1.,0.965925826289068,1.,0.965925826289068,1.,0.965925826289068,
1.,0.965925826289068,1.,0.965925826289068,1.,0.965925826289068,1.,0.965925826289068,
1.,0.965925826289068,1.,0.965925826289068,1.,0.965925826289068,1.,0.965925826289068,
1.,0.965925826289068,1.,0.965925826289068,1.,0.965925826289068,1.,0.965925826289068,
1.,0.965925826289068,1.,0.965925826289068,1.,0.965925826289068,1.,0.965925826289068,
1.,0.965925826289068,1.,0.965925826289068,1.,0.965925826289068,1.,0.965925826289068,
1.,0.965925826289068,1.,0.965925826289068,1.,0.965925826289068,1.,0.965925826289068,
1.,0.965925826289068,1.,0.965925826289068,1.,0.965925826289068,1.,0.965925826289068,
1.,0.965925826289068,1.,0.965925826289068,1.,0.965925826289068,1.,0.965925826289068,
1.,0.965925826289068,1.,0.965925826289068,1.),(1.,0.965925826289068,1.,
0.965925826289068,1.,0.965925826289068,1.,0.965925826289068,1.,0.965925826289068,
1.,0.965925826289068,1.,0.965925826289068,1.,0.965925826289068,1.,0.965925826289068,
1.,0.965925826289068,1.,0.965925826289068,1.,0.965925826289068,1.,0.965925826289068,
1.,0.965925826289068,1.,0.965925826289068,1.,0.965925826289068,1.,0.965925826289068,
1.,0.965925826289068,1.,0.965925826289068,1.,0.965925826289068,1.,0.965925826289068,
1.,0.965925826289068,1.,0.965925826289068,1.,0.965925826289068,1.,0.965925826289068,
1.,0.965925826289068,1.,0.965925826289068,1.,0.965925826289068,1.,0.965925826289068,
1.,0.965925826289068,1.,0.965925826289068,1.,0.965925826289068,1.,0.965925826289068,
1.,0.965925826289068,1.,0.965925826289068,1.,0.965925826289068,1.,0.965925826289068,
1.,0.965925826289068,1.,0.965925826289068,1.,0.965925826289068,1.,0.965925826289068,
1.,0.965925826289068,1.,0.965925826289068,1.,0.965925826289068,1.,0.965925826289068,
1.,0.965925826289068,1.,0.965925826289068,1.,0.965925826289068,1.,0.965925826289068,
1.,0.965925826289068,1.,0.965925826289068,1.,0.965925826289068,1.,0.965925826289068,
1.,0.965925826289068,1.,0.965925826289068,1.,0.965925826289068,1.,0.965925826289068,
1.,0.965925826289068,1.,0.965925826289068,1.,0.965925826289068,1.,0.965925826289068,
1.,0.965925826289068,1.,0.965925826289068,1.,0.965925826289068,1.,0.965925826289068,
1.,0.965925826289068,1.,0.965925826289068,1.,0.965925826289068,1.,0.965925826289068,
1.,0.965925826289068,1.,0.965925826289068,1.,0.965925826289068,1.)))
REPRESENTATION_ITEM('')
SURFACE()
);
#161=(
BOUNDED_SURFACE()
B_SPLINE_SURFACE(1,2,((#8344,#8345,#8346,#8347,#8348,#8349,#8350,#8351,
#8352,#8353,#8354,#8355,#8356,#8357,#8358,#8359,#8360,#8361,#8362,#8363,
#8364,#8365,#8366,#8367,#8368,#8369,#8370,#8371,#8372,#8373,#8374,#8375,
#8376,#8377,#8378,#8379,#8380,#8381,#8382,#8383,#8384,#8385,#8386,#8387,
#8388,#8389,#8390,#8391,#8392,#8393,#8394,#8395,#8396,#8397,#8398,#8399,
#8400,#8401,#8402,#8403,#8404,#8405,#8406,#8407,#8408,#8409,#8410,#8411,
#8412,#8413,#8414,#8415,#8416,#8417,#8418,#8419,#8420,#8421,#8422,#8423,
#8424,#8425,#8426,#8427,#8428,#8429,#8430,#8431,#8432,#8433,#8434,#8435,
#8436,#8437,#8438,#8439,#8440,#8441,#8442,#8443,#8444,#8445,#8446,#8447,
#8448,#8449,#8450,#8451,#8452,#8453,#8454,#8455,#8456,#8457,#8458,#8459,
#8460,#8461,#8462,#8463,#8464,#8465,#8466,#8467,#8468,#8469,#8470,#8471,
#8472,#8473,#8474,#8475,#8476,#8477,#8478,#8479,#8480,#8481,#8482,#8483,
#8484,#8485,#8486,#8487,#8488),(#8489,#8490,#8491,#8492,#8493,#8494,#8495,
#8496,#8497,#8498,#8499,#8500,#8501,#8502,#8503,#8504,#8505,#8506,#8507,
#8508,#8509,#8510,#8511,#8512,#8513,#8514,#8515,#8516,#8517,#8518,#8519,
#8520,#8521,#8522,#8523,#8524,#8525,#8526,#8527,#8528,#8529,#8530,#8531,
#8532,#8533,#8534,#8535,#8536,#8537,#8538,#8539,#8540,#8541,#8542,#8543,
#8544,#8545,#8546,#8547,#8548,#8549,#8550,#8551,#8552,#8553,#8554,#8555,
#8556,#8557,#8558,#8559,#8560,#8561,#8562,#8563,#8564,#8565,#8566,#8567,
#8568,#8569,#8570,#8571,#8572,#8573,#8574,#8575,#8576,#8577,#8578,#8579,
#8580,#8581,#8582,#8583,#8584,#8585,#8586,#8587,#8588,#8589,#8590,#8591,
#8592,#8593,#8594,#8595,#8596,#8597,#8598,#8599,#8600,#8601,#8602,#8603,
#8604,#8605,#8606,#8607,#8608,#8609,#8610,#8611,#8612,#8613,#8614,#8615,
#8616,#8617,#8618,#8619,#8620,#8621,#8622,#8623,#8624,#8625,#8626,#8627,
#8628,#8629,#8630,#8631,#8632,#8633)),.UNSPECIFIED.,.F.,.F.,.F.)
B_SPLINE_SURFACE_WITH_KNOTS((2,2),(3,2,2,2,2,2,2,2,2,2,2,2,2,2,2,2,2,2,
2,2,2,2,2,2,2,2,2,2,2,2,2,2,2,2,2,2,2,2,2,2,2,2,2,2,2,2,2,2,2,2,2,2,2,2,
2,2,2,2,2,2,2,2,2,2,2,2,2,2,2,2,2,2,3),(0.,1.),(0.,0.0138888888888889,0.0277777777777778,
0.0416666666666667,0.0555555555555556,0.0694444444444444,0.0833333333333333,
0.0972222222222222,0.111111111111111,0.125,0.138888888888889,0.152777777777778,
0.166666666666667,0.180555555555556,0.194444444444444,0.208333333333333,
0.222222222222222,0.236111111111111,0.25,0.263888888888889,0.277777777777778,
0.291666666666667,0.305555555555556,0.319444444444444,0.333333333333333,
0.347222222222222,0.361111111111111,0.375,0.388888888888889,0.402777777777778,
0.416666666666667,0.430555555555556,0.444444444444444,0.458333333333333,
0.472222222222222,0.486111111111111,0.5,0.513888888888889,0.527777777777778,
0.541666666666667,0.555555555555556,0.569444444444444,0.583333333333333,
0.597222222222222,0.611111111111111,0.625,0.638888888888889,0.652777777777778,
0.666666666666667,0.680555555555556,0.694444444444444,0.708333333333333,
0.722222222222222,0.736111111111111,0.75,0.763888888888889,0.777777777777778,
0.791666666666667,0.805555555555556,0.819444444444444,0.833333333333333,
0.847222222222222,0.861111111111111,0.875,0.888888888888889,0.902777777777778,
0.916666666666667,0.930555555555556,0.944444444444444,0.958333333333333,
0.972222222222222,0.986111111111111,1.),.UNSPECIFIED.)
GEOMETRIC_REPRESENTATION_ITEM()
RATIONAL_B_SPLINE_SURFACE(((1.,0.965925826289068,1.,0.965925826289068,1.,
0.965925826289068,1.,0.965925826289068,1.,0.965925826289068,1.,0.965925826289068,
1.,0.965925826289068,1.,0.965925826289068,1.,0.965925826289068,1.,0.965925826289068,
1.,0.965925826289068,1.,0.965925826289068,1.,0.965925826289068,1.,0.965925826289068,
1.,0.965925826289068,1.,0.965925826289068,1.,0.965925826289068,1.,0.965925826289068,
1.,0.965925826289068,1.,0.965925826289068,1.,0.965925826289068,1.,0.965925826289068,
1.,0.965925826289068,1.,0.965925826289068,1.,0.965925826289068,1.,0.965925826289068,
1.,0.965925826289068,1.,0.965925826289068,1.,0.965925826289068,1.,0.965925826289068,
1.,0.965925826289068,1.,0.965925826289068,1.,0.965925826289068,1.,0.965925826289068,
1.,0.965925826289068,1.,0.965925826289068,1.,0.965925826289068,1.,0.965925826289068,
1.,0.965925826289068,1.,0.965925826289068,1.,0.965925826289068,1.,0.965925826289068,
1.,0.965925826289068,1.,0.965925826289068,1.,0.965925826289068,1.,0.965925826289068,
1.,0.965925826289068,1.,0.965925826289068,1.,0.965925826289068,1.,0.965925826289068,
1.,0.965925826289068,1.,0.965925826289068,1.,0.965925826289068,1.,0.965925826289068,
1.,0.965925826289068,1.,0.965925826289068,1.,0.965925826289068,1.,0.965925826289068,
1.,0.965925826289068,1.,0.965925826289068,1.,0.965925826289068,1.,0.965925826289068,
1.,0.965925826289068,1.,0.965925826289068,1.,0.965925826289068,1.,0.965925826289068,
1.,0.965925826289068,1.,0.965925826289068,1.,0.965925826289068,1.,0.965925826289068,
1.,0.965925826289068,1.,0.965925826289068,1.),(1.,0.965925826289068,1.,
0.965925826289068,1.,0.965925826289068,1.,0.965925826289068,1.,0.965925826289068,
1.,0.965925826289068,1.,0.965925826289068,1.,0.965925826289068,1.,0.965925826289068,
1.,0.965925826289068,1.,0.965925826289068,1.,0.965925826289068,1.,0.965925826289068,
1.,0.965925826289068,1.,0.965925826289068,1.,0.965925826289068,1.,0.965925826289068,
1.,0.965925826289068,1.,0.965925826289068,1.,0.965925826289068,1.,0.965925826289068,
1.,0.965925826289068,1.,0.965925826289068,1.,0.965925826289068,1.,0.965925826289068,
1.,0.965925826289068,1.,0.965925826289068,1.,0.965925826289068,1.,0.965925826289068,
1.,0.965925826289068,1.,0.965925826289068,1.,0.965925826289068,1.,0.965925826289068,
1.,0.965925826289068,1.,0.965925826289068,1.,0.965925826289068,1.,0.965925826289068,
1.,0.965925826289068,1.,0.965925826289068,1.,0.965925826289068,1.,0.965925826289068,
1.,0.965925826289068,1.,0.965925826289068,1.,0.965925826289068,1.,0.965925826289068,
1.,0.965925826289068,1.,0.965925826289068,1.,0.965925826289068,1.,0.965925826289068,
1.,0.965925826289068,1.,0.965925826289068,1.,0.965925826289068,1.,0.965925826289068,
1.,0.965925826289068,1.,0.965925826289068,1.,0.965925826289068,1.,0.965925826289068,
1.,0.965925826289068,1.,0.965925826289068,1.,0.965925826289068,1.,0.965925826289068,
1.,0.965925826289068,1.,0.965925826289068,1.,0.965925826289068,1.,0.965925826289068,
1.,0.965925826289068,1.,0.965925826289068,1.,0.965925826289068,1.,0.965925826289068,
1.,0.965925826289068,1.,0.965925826289068,1.,0.965925826289068,1.)))
REPRESENTATION_ITEM('')
SURFACE()
);
#162=(
BOUNDED_SURFACE()
B_SPLINE_SURFACE(1,2,((#8651,#8652,#8653,#8654,#8655,#8656,#8657,#8658,
#8659,#8660,#8661,#8662,#8663,#8664,#8665,#8666,#8667,#8668,#8669,#8670,
#8671,#8672,#8673,#8674,#8675,#8676,#8677,#8678,#8679,#8680,#8681,#8682,
#8683,#8684,#8685,#8686,#8687,#8688,#8689,#8690,#8691,#8692,#8693,#8694,
#8695,#8696,#8697,#8698,#8699,#8700,#8701,#8702,#8703,#8704,#8705,#8706,
#8707,#8708,#8709,#8710,#8711,#8712,#8713,#8714,#8715,#8716,#8717,#8718,
#8719,#8720,#8721,#8722,#8723,#8724,#8725,#8726,#8727,#8728,#8729,#8730,
#8731,#8732,#8733,#8734,#8735,#8736,#8737,#8738,#8739,#8740,#8741,#8742,
#8743,#8744,#8745,#8746,#8747,#8748,#8749,#8750,#8751,#8752,#8753,#8754,
#8755,#8756,#8757,#8758,#8759,#8760,#8761,#8762,#8763,#8764,#8765,#8766,
#8767,#8768,#8769,#8770,#8771,#8772,#8773,#8774,#8775,#8776,#8777,#8778,
#8779,#8780,#8781,#8782,#8783,#8784,#8785,#8786,#8787,#8788,#8789,#8790,
#8791,#8792,#8793,#8794,#8795),(#8796,#8797,#8798,#8799,#8800,#8801,#8802,
#8803,#8804,#8805,#8806,#8807,#8808,#8809,#8810,#8811,#8812,#8813,#8814,
#8815,#8816,#8817,#8818,#8819,#8820,#8821,#8822,#8823,#8824,#8825,#8826,
#8827,#8828,#8829,#8830,#8831,#8832,#8833,#8834,#8835,#8836,#8837,#8838,
#8839,#8840,#8841,#8842,#8843,#8844,#8845,#8846,#8847,#8848,#8849,#8850,
#8851,#8852,#8853,#8854,#8855,#8856,#8857,#8858,#8859,#8860,#8861,#8862,
#8863,#8864,#8865,#8866,#8867,#8868,#8869,#8870,#8871,#8872,#8873,#8874,
#8875,#8876,#8877,#8878,#8879,#8880,#8881,#8882,#8883,#8884,#8885,#8886,
#8887,#8888,#8889,#8890,#8891,#8892,#8893,#8894,#8895,#8896,#8897,#8898,
#8899,#8900,#8901,#8902,#8903,#8904,#8905,#8906,#8907,#8908,#8909,#8910,
#8911,#8912,#8913,#8914,#8915,#8916,#8917,#8918,#8919,#8920,#8921,#8922,
#8923,#8924,#8925,#8926,#8927,#8928,#8929,#8930,#8931,#8932,#8933,#8934,
#8935,#8936,#8937,#8938,#8939,#8940)),.UNSPECIFIED.,.F.,.F.,.F.)
B_SPLINE_SURFACE_WITH_KNOTS((2,2),(3,2,2,2,2,2,2,2,2,2,2,2,2,2,2,2,2,2,
2,2,2,2,2,2,2,2,2,2,2,2,2,2,2,2,2,2,2,2,2,2,2,2,2,2,2,2,2,2,2,2,2,2,2,2,
2,2,2,2,2,2,2,2,2,2,2,2,2,2,2,2,2,2,3),(0.,1.),(0.,0.0138888888888889,0.0277777777777778,
0.0416666666666667,0.0555555555555556,0.0694444444444444,0.0833333333333333,
0.0972222222222222,0.111111111111111,0.125,0.138888888888889,0.152777777777778,
0.166666666666667,0.180555555555556,0.194444444444444,0.208333333333333,
0.222222222222222,0.236111111111111,0.25,0.263888888888889,0.277777777777778,
0.291666666666667,0.305555555555556,0.319444444444444,0.333333333333333,
0.347222222222222,0.361111111111111,0.375,0.388888888888889,0.402777777777778,
0.416666666666667,0.430555555555556,0.444444444444444,0.458333333333333,
0.472222222222222,0.486111111111111,0.5,0.513888888888889,0.527777777777778,
0.541666666666667,0.555555555555556,0.569444444444444,0.583333333333333,
0.597222222222222,0.611111111111111,0.625,0.638888888888889,0.652777777777778,
0.666666666666667,0.680555555555556,0.694444444444444,0.708333333333333,
0.722222222222222,0.736111111111111,0.75,0.763888888888889,0.777777777777778,
0.791666666666667,0.805555555555556,0.819444444444444,0.833333333333333,
0.847222222222222,0.861111111111111,0.875,0.888888888888889,0.902777777777778,
0.916666666666667,0.930555555555556,0.944444444444444,0.958333333333333,
0.972222222222222,0.986111111111111,1.),.UNSPECIFIED.)
GEOMETRIC_REPRESENTATION_ITEM()
RATIONAL_B_SPLINE_SURFACE(((1.,0.965925826289068,1.,0.965925826289068,1.,
0.965925826289068,1.,0.965925826289068,1.,0.965925826289068,1.,0.965925826289068,
1.,0.965925826289068,1.,0.965925826289068,1.,0.965925826289068,1.,0.965925826289068,
1.,0.965925826289068,1.,0.965925826289068,1.,0.965925826289068,1.,0.965925826289068,
1.,0.965925826289068,1.,0.965925826289068,1.,0.965925826289068,1.,0.965925826289068,
1.,0.965925826289068,1.,0.965925826289068,1.,0.965925826289068,1.,0.965925826289068,
1.,0.965925826289068,1.,0.965925826289068,1.,0.965925826289068,1.,0.965925826289068,
1.,0.965925826289068,1.,0.965925826289068,1.,0.965925826289068,1.,0.965925826289068,
1.,0.965925826289068,1.,0.965925826289068,1.,0.965925826289068,1.,0.965925826289068,
1.,0.965925826289068,1.,0.965925826289068,1.,0.965925826289068,1.,0.965925826289068,
1.,0.965925826289068,1.,0.965925826289068,1.,0.965925826289068,1.,0.965925826289068,
1.,0.965925826289068,1.,0.965925826289068,1.,0.965925826289068,1.,0.965925826289068,
1.,0.965925826289068,1.,0.965925826289068,1.,0.965925826289068,1.,0.965925826289068,
1.,0.965925826289068,1.,0.965925826289068,1.,0.965925826289068,1.,0.965925826289068,
1.,0.965925826289068,1.,0.965925826289068,1.,0.965925826289068,1.,0.965925826289068,
1.,0.965925826289068,1.,0.965925826289068,1.,0.965925826289068,1.,0.965925826289068,
1.,0.965925826289068,1.,0.965925826289068,1.,0.965925826289068,1.,0.965925826289068,
1.,0.965925826289068,1.,0.965925826289068,1.,0.965925826289068,1.,0.965925826289068,
1.,0.965925826289068,1.,0.965925826289068,1.),(1.,0.965925826289068,1.,
0.965925826289068,1.,0.965925826289068,1.,0.965925826289068,1.,0.965925826289068,
1.,0.965925826289068,1.,0.965925826289068,1.,0.965925826289068,1.,0.965925826289068,
1.,0.965925826289068,1.,0.965925826289068,1.,0.965925826289068,1.,0.965925826289068,
1.,0.965925826289068,1.,0.965925826289068,1.,0.965925826289068,1.,0.965925826289068,
1.,0.965925826289068,1.,0.965925826289068,1.,0.965925826289068,1.,0.965925826289068,
1.,0.965925826289068,1.,0.965925826289068,1.,0.965925826289068,1.,0.965925826289068,
1.,0.965925826289068,1.,0.965925826289068,1.,0.965925826289068,1.,0.965925826289068,
1.,0.965925826289068,1.,0.965925826289068,1.,0.965925826289068,1.,0.965925826289068,
1.,0.965925826289068,1.,0.965925826289068,1.,0.965925826289068,1.,0.965925826289068,
1.,0.965925826289068,1.,0.965925826289068,1.,0.965925826289068,1.,0.965925826289068,
1.,0.965925826289068,1.,0.965925826289068,1.,0.965925826289068,1.,0.965925826289068,
1.,0.965925826289068,1.,0.965925826289068,1.,0.965925826289068,1.,0.965925826289068,
1.,0.965925826289068,1.,0.965925826289068,1.,0.965925826289068,1.,0.965925826289068,
1.,0.965925826289068,1.,0.965925826289068,1.,0.965925826289068,1.,0.965925826289068,
1.,0.965925826289068,1.,0.965925826289068,1.,0.965925826289068,1.,0.965925826289068,
1.,0.965925826289068,1.,0.965925826289068,1.,0.965925826289068,1.,0.965925826289068,
1.,0.965925826289068,1.,0.965925826289068,1.,0.965925826289068,1.,0.965925826289068,
1.,0.965925826289068,1.,0.965925826289068,1.,0.965925826289068,1.)))
REPRESENTATION_ITEM('')
SURFACE()
);
#163=(
BOUNDED_SURFACE()
B_SPLINE_SURFACE(1,2,((#8966,#8967,#8968,#8969,#8970,#8971,#8972,#8973,
#8974,#8975,#8976,#8977,#8978,#8979,#8980,#8981,#8982,#8983,#8984,#8985,
#8986,#8987,#8988,#8989,#8990,#8991,#8992,#8993,#8994,#8995,#8996,#8997,
#8998,#8999,#9000,#9001,#9002,#9003,#9004,#9005,#9006,#9007,#9008,#9009,
#9010,#9011,#9012,#9013,#9014,#9015,#9016,#9017,#9018,#9019,#9020,#9021,
#9022,#9023,#9024,#9025,#9026,#9027,#9028,#9029,#9030,#9031,#9032,#9033,
#9034,#9035,#9036,#9037,#9038,#9039,#9040,#9041,#9042,#9043,#9044,#9045,
#9046,#9047,#9048,#9049,#9050,#9051,#9052,#9053,#9054,#9055,#9056,#9057,
#9058,#9059,#9060,#9061,#9062,#9063,#9064,#9065,#9066,#9067,#9068,#9069,
#9070,#9071,#9072,#9073,#9074,#9075,#9076,#9077,#9078,#9079,#9080,#9081,
#9082,#9083,#9084,#9085,#9086,#9087,#9088,#9089,#9090,#9091,#9092,#9093,
#9094,#9095,#9096,#9097,#9098,#9099,#9100,#9101,#9102,#9103,#9104,#9105,
#9106,#9107,#9108,#9109,#9110),(#9111,#9112,#9113,#9114,#9115,#9116,#9117,
#9118,#9119,#9120,#9121,#9122,#9123,#9124,#9125,#9126,#9127,#9128,#9129,
#9130,#9131,#9132,#9133,#9134,#9135,#9136,#9137,#9138,#9139,#9140,#9141,
#9142,#9143,#9144,#9145,#9146,#9147,#9148,#9149,#9150,#9151,#9152,#9153,
#9154,#9155,#9156,#9157,#9158,#9159,#9160,#9161,#9162,#9163,#9164,#9165,
#9166,#9167,#9168,#9169,#9170,#9171,#9172,#9173,#9174,#9175,#9176,#9177,
#9178,#9179,#9180,#9181,#9182,#9183,#9184,#9185,#9186,#9187,#9188,#9189,
#9190,#9191,#9192,#9193,#9194,#9195,#9196,#9197,#9198,#9199,#9200,#9201,
#9202,#9203,#9204,#9205,#9206,#9207,#9208,#9209,#9210,#9211,#9212,#9213,
#9214,#9215,#9216,#9217,#9218,#9219,#9220,#9221,#9222,#9223,#9224,#9225,
#9226,#9227,#9228,#9229,#9230,#9231,#9232,#9233,#9234,#9235,#9236,#9237,
#9238,#9239,#9240,#9241,#9242,#9243,#9244,#9245,#9246,#9247,#9248,#9249,
#9250,#9251,#9252,#9253,#9254,#9255)),.UNSPECIFIED.,.F.,.F.,.F.)
B_SPLINE_SURFACE_WITH_KNOTS((2,2),(3,2,2,2,2,2,2,2,2,2,2,2,2,2,2,2,2,2,
2,2,2,2,2,2,2,2,2,2,2,2,2,2,2,2,2,2,2,2,2,2,2,2,2,2,2,2,2,2,2,2,2,2,2,2,
2,2,2,2,2,2,2,2,2,2,2,2,2,2,2,2,2,2,3),(0.,1.),(0.,0.0138888888888889,0.0277777777777778,
0.0416666666666667,0.0555555555555556,0.0694444444444444,0.0833333333333333,
0.0972222222222222,0.111111111111111,0.125,0.138888888888889,0.152777777777778,
0.166666666666667,0.180555555555556,0.194444444444444,0.208333333333333,
0.222222222222222,0.236111111111111,0.25,0.263888888888889,0.277777777777778,
0.291666666666667,0.305555555555556,0.319444444444444,0.333333333333333,
0.347222222222222,0.361111111111111,0.375,0.388888888888889,0.402777777777778,
0.416666666666667,0.430555555555556,0.444444444444444,0.458333333333333,
0.472222222222222,0.486111111111111,0.5,0.513888888888889,0.527777777777778,
0.541666666666667,0.555555555555556,0.569444444444444,0.583333333333333,
0.597222222222222,0.611111111111111,0.625,0.638888888888889,0.652777777777778,
0.666666666666667,0.680555555555556,0.694444444444444,0.708333333333333,
0.722222222222222,0.736111111111111,0.75,0.763888888888889,0.777777777777778,
0.791666666666667,0.805555555555556,0.819444444444444,0.833333333333333,
0.847222222222222,0.861111111111111,0.875,0.888888888888889,0.902777777777778,
0.916666666666667,0.930555555555556,0.944444444444444,0.958333333333333,
0.972222222222222,0.986111111111111,1.),.UNSPECIFIED.)
GEOMETRIC_REPRESENTATION_ITEM()
RATIONAL_B_SPLINE_SURFACE(((1.,0.965925826289068,1.,0.965925826289068,1.,
0.965925826289068,1.,0.965925826289068,1.,0.965925826289068,1.,0.965925826289068,
1.,0.965925826289068,1.,0.965925826289068,1.,0.965925826289068,1.,0.965925826289068,
1.,0.965925826289068,1.,0.965925826289068,1.,0.965925826289068,1.,0.965925826289068,
1.,0.965925826289068,1.,0.965925826289068,1.,0.965925826289068,1.,0.965925826289068,
1.,0.965925826289068,1.,0.965925826289068,1.,0.965925826289068,1.,0.965925826289068,
1.,0.965925826289068,1.,0.965925826289068,1.,0.965925826289068,1.,0.965925826289068,
1.,0.965925826289068,1.,0.965925826289068,1.,0.965925826289068,1.,0.965925826289068,
1.,0.965925826289068,1.,0.965925826289068,1.,0.965925826289068,1.,0.965925826289068,
1.,0.965925826289068,1.,0.965925826289068,1.,0.965925826289068,1.,0.965925826289068,
1.,0.965925826289068,1.,0.965925826289068,1.,0.965925826289068,1.,0.965925826289068,
1.,0.965925826289068,1.,0.965925826289068,1.,0.965925826289068,1.,0.965925826289068,
1.,0.965925826289068,1.,0.965925826289068,1.,0.965925826289068,1.,0.965925826289068,
1.,0.965925826289068,1.,0.965925826289068,1.,0.965925826289068,1.,0.965925826289068,
1.,0.965925826289068,1.,0.965925826289068,1.,0.965925826289068,1.,0.965925826289068,
1.,0.965925826289068,1.,0.965925826289068,1.,0.965925826289068,1.,0.965925826289068,
1.,0.965925826289068,1.,0.965925826289068,1.,0.965925826289068,1.,0.965925826289068,
1.,0.965925826289068,1.,0.965925826289068,1.,0.965925826289068,1.,0.965925826289068,
1.,0.965925826289068,1.,0.965925826289068,1.),(1.,0.965925826289068,1.,
0.965925826289068,1.,0.965925826289068,1.,0.965925826289068,1.,0.965925826289068,
1.,0.965925826289068,1.,0.965925826289068,1.,0.965925826289068,1.,0.965925826289068,
1.,0.965925826289068,1.,0.965925826289068,1.,0.965925826289068,1.,0.965925826289068,
1.,0.965925826289068,1.,0.965925826289068,1.,0.965925826289068,1.,0.965925826289068,
1.,0.965925826289068,1.,0.965925826289068,1.,0.965925826289068,1.,0.965925826289068,
1.,0.965925826289068,1.,0.965925826289068,1.,0.965925826289068,1.,0.965925826289068,
1.,0.965925826289068,1.,0.965925826289068,1.,0.965925826289068,1.,0.965925826289068,
1.,0.965925826289068,1.,0.965925826289068,1.,0.965925826289068,1.,0.965925826289068,
1.,0.965925826289068,1.,0.965925826289068,1.,0.965925826289068,1.,0.965925826289068,
1.,0.965925826289068,1.,0.965925826289068,1.,0.965925826289068,1.,0.965925826289068,
1.,0.965925826289068,1.,0.965925826289068,1.,0.965925826289068,1.,0.965925826289068,
1.,0.965925826289068,1.,0.965925826289068,1.,0.965925826289068,1.,0.965925826289068,
1.,0.965925826289068,1.,0.965925826289068,1.,0.965925826289068,1.,0.965925826289068,
1.,0.965925826289068,1.,0.965925826289068,1.,0.965925826289068,1.,0.965925826289068,
1.,0.965925826289068,1.,0.965925826289068,1.,0.965925826289068,1.,0.965925826289068,
1.,0.965925826289068,1.,0.965925826289068,1.,0.965925826289068,1.,0.965925826289068,
1.,0.965925826289068,1.,0.965925826289068,1.,0.965925826289068,1.,0.965925826289068,
1.,0.965925826289068,1.,0.965925826289068,1.,0.965925826289068,1.)))
REPRESENTATION_ITEM('')
SURFACE()
);
#164=(
BOUNDED_SURFACE()
B_SPLINE_SURFACE(1,2,((#9273,#9274,#9275,#9276,#9277,#9278,#9279,#9280,
#9281,#9282,#9283,#9284,#9285,#9286,#9287,#9288,#9289,#9290,#9291,#9292,
#9293,#9294,#9295,#9296,#9297,#9298,#9299,#9300,#9301,#9302,#9303,#9304,
#9305,#9306,#9307,#9308,#9309,#9310,#9311,#9312,#9313,#9314,#9315,#9316,
#9317,#9318,#9319,#9320,#9321,#9322,#9323,#9324,#9325,#9326,#9327,#9328,
#9329,#9330,#9331,#9332,#9333,#9334,#9335,#9336,#9337,#9338,#9339,#9340,
#9341,#9342,#9343,#9344,#9345,#9346,#9347,#9348,#9349,#9350,#9351,#9352,
#9353,#9354,#9355,#9356,#9357,#9358,#9359,#9360,#9361,#9362,#9363,#9364,
#9365,#9366,#9367,#9368,#9369,#9370,#9371,#9372,#9373,#9374,#9375,#9376,
#9377,#9378,#9379,#9380,#9381,#9382,#9383,#9384,#9385,#9386,#9387,#9388,
#9389,#9390,#9391,#9392,#9393,#9394,#9395,#9396,#9397,#9398,#9399,#9400,
#9401,#9402,#9403,#9404,#9405,#9406,#9407,#9408,#9409,#9410,#9411,#9412,
#9413,#9414,#9415,#9416,#9417),(#9418,#9419,#9420,#9421,#9422,#9423,#9424,
#9425,#9426,#9427,#9428,#9429,#9430,#9431,#9432,#9433,#9434,#9435,#9436,
#9437,#9438,#9439,#9440,#9441,#9442,#9443,#9444,#9445,#9446,#9447,#9448,
#9449,#9450,#9451,#9452,#9453,#9454,#9455,#9456,#9457,#9458,#9459,#9460,
#9461,#9462,#9463,#9464,#9465,#9466,#9467,#9468,#9469,#9470,#9471,#9472,
#9473,#9474,#9475,#9476,#9477,#9478,#9479,#9480,#9481,#9482,#9483,#9484,
#9485,#9486,#9487,#9488,#9489,#9490,#9491,#9492,#9493,#9494,#9495,#9496,
#9497,#9498,#9499,#9500,#9501,#9502,#9503,#9504,#9505,#9506,#9507,#9508,
#9509,#9510,#9511,#9512,#9513,#9514,#9515,#9516,#9517,#9518,#9519,#9520,
#9521,#9522,#9523,#9524,#9525,#9526,#9527,#9528,#9529,#9530,#9531,#9532,
#9533,#9534,#9535,#9536,#9537,#9538,#9539,#9540,#9541,#9542,#9543,#9544,
#9545,#9546,#9547,#9548,#9549,#9550,#9551,#9552,#9553,#9554,#9555,#9556,
#9557,#9558,#9559,#9560,#9561,#9562)),.UNSPECIFIED.,.F.,.F.,.F.)
B_SPLINE_SURFACE_WITH_KNOTS((2,2),(3,2,2,2,2,2,2,2,2,2,2,2,2,2,2,2,2,2,
2,2,2,2,2,2,2,2,2,2,2,2,2,2,2,2,2,2,2,2,2,2,2,2,2,2,2,2,2,2,2,2,2,2,2,2,
2,2,2,2,2,2,2,2,2,2,2,2,2,2,2,2,2,2,3),(0.,1.),(0.,0.0138888888888889,0.0277777777777778,
0.0416666666666667,0.0555555555555556,0.0694444444444444,0.0833333333333333,
0.0972222222222222,0.111111111111111,0.125,0.138888888888889,0.152777777777778,
0.166666666666667,0.180555555555556,0.194444444444444,0.208333333333333,
0.222222222222222,0.236111111111111,0.25,0.263888888888889,0.277777777777778,
0.291666666666667,0.305555555555556,0.319444444444444,0.333333333333333,
0.347222222222222,0.361111111111111,0.375,0.388888888888889,0.402777777777778,
0.416666666666667,0.430555555555556,0.444444444444444,0.458333333333333,
0.472222222222222,0.486111111111111,0.5,0.513888888888889,0.527777777777778,
0.541666666666667,0.555555555555556,0.569444444444444,0.583333333333333,
0.597222222222222,0.611111111111111,0.625,0.638888888888889,0.652777777777778,
0.666666666666667,0.680555555555556,0.694444444444444,0.708333333333333,
0.722222222222222,0.736111111111111,0.75,0.763888888888889,0.777777777777778,
0.791666666666667,0.805555555555556,0.819444444444444,0.833333333333333,
0.847222222222222,0.861111111111111,0.875,0.888888888888889,0.902777777777778,
0.916666666666667,0.930555555555556,0.944444444444444,0.958333333333333,
0.972222222222222,0.986111111111111,1.),.UNSPECIFIED.)
GEOMETRIC_REPRESENTATION_ITEM()
RATIONAL_B_SPLINE_SURFACE(((1.,0.965925826289068,1.,0.965925826289068,1.,
0.965925826289068,1.,0.965925826289068,1.,0.965925826289068,1.,0.965925826289068,
1.,0.965925826289068,1.,0.965925826289068,1.,0.965925826289068,1.,0.965925826289068,
1.,0.965925826289068,1.,0.965925826289068,1.,0.965925826289068,1.,0.965925826289068,
1.,0.965925826289068,1.,0.965925826289068,1.,0.965925826289068,1.,0.965925826289068,
1.,0.965925826289068,1.,0.965925826289068,1.,0.965925826289068,1.,0.965925826289068,
1.,0.965925826289068,1.,0.965925826289068,1.,0.965925826289068,1.,0.965925826289068,
1.,0.965925826289068,1.,0.965925826289068,1.,0.965925826289068,1.,0.965925826289068,
1.,0.965925826289068,1.,0.965925826289068,1.,0.965925826289068,1.,0.965925826289068,
1.,0.965925826289068,1.,0.965925826289068,1.,0.965925826289068,1.,0.965925826289068,
1.,0.965925826289068,1.,0.965925826289068,1.,0.965925826289068,1.,0.965925826289068,
1.,0.965925826289068,1.,0.965925826289068,1.,0.965925826289068,1.,0.965925826289068,
1.,0.965925826289068,1.,0.965925826289068,1.,0.965925826289068,1.,0.965925826289068,
1.,0.965925826289068,1.,0.965925826289068,1.,0.965925826289068,1.,0.965925826289068,
1.,0.965925826289068,1.,0.965925826289068,1.,0.965925826289068,1.,0.965925826289068,
1.,0.965925826289068,1.,0.965925826289068,1.,0.965925826289068,1.,0.965925826289068,
1.,0.965925826289068,1.,0.965925826289068,1.,0.965925826289068,1.,0.965925826289068,
1.,0.965925826289068,1.,0.965925826289068,1.,0.965925826289068,1.,0.965925826289068,
1.,0.965925826289068,1.,0.965925826289068,1.),(1.,0.965925826289068,1.,
0.965925826289068,1.,0.965925826289068,1.,0.965925826289068,1.,0.965925826289068,
1.,0.965925826289068,1.,0.965925826289068,1.,0.965925826289068,1.,0.965925826289068,
1.,0.965925826289068,1.,0.965925826289068,1.,0.965925826289068,1.,0.965925826289068,
1.,0.965925826289068,1.,0.965925826289068,1.,0.965925826289068,1.,0.965925826289068,
1.,0.965925826289068,1.,0.965925826289068,1.,0.965925826289068,1.,0.965925826289068,
1.,0.965925826289068,1.,0.965925826289068,1.,0.965925826289068,1.,0.965925826289068,
1.,0.965925826289068,1.,0.965925826289068,1.,0.965925826289068,1.,0.965925826289068,
1.,0.965925826289068,1.,0.965925826289068,1.,0.965925826289068,1.,0.965925826289068,
1.,0.965925826289068,1.,0.965925826289068,1.,0.965925826289068,1.,0.965925826289068,
1.,0.965925826289068,1.,0.965925826289068,1.,0.965925826289068,1.,0.965925826289068,
1.,0.965925826289068,1.,0.965925826289068,1.,0.965925826289068,1.,0.965925826289068,
1.,0.965925826289068,1.,0.965925826289068,1.,0.965925826289068,1.,0.965925826289068,
1.,0.965925826289068,1.,0.965925826289068,1.,0.965925826289068,1.,0.965925826289068,
1.,0.965925826289068,1.,0.965925826289068,1.,0.965925826289068,1.,0.965925826289068,
1.,0.965925826289068,1.,0.965925826289068,1.,0.965925826289068,1.,0.965925826289068,
1.,0.965925826289068,1.,0.965925826289068,1.,0.965925826289068,1.,0.965925826289068,
1.,0.965925826289068,1.,0.965925826289068,1.,0.965925826289068,1.,0.965925826289068,
1.,0.965925826289068,1.,0.965925826289068,1.,0.965925826289068,1.)))
REPRESENTATION_ITEM('')
SURFACE()
);
#165=(
BOUNDED_SURFACE()
B_SPLINE_SURFACE(1,2,((#9588,#9589,#9590,#9591,#9592,#9593,#9594,#9595,
#9596,#9597,#9598,#9599,#9600,#9601,#9602,#9603,#9604,#9605,#9606,#9607,
#9608,#9609,#9610,#9611,#9612,#9613,#9614,#9615,#9616,#9617,#9618,#9619,
#9620,#9621,#9622,#9623,#9624,#9625,#9626,#9627,#9628,#9629,#9630,#9631,
#9632,#9633,#9634,#9635,#9636,#9637,#9638,#9639,#9640,#9641,#9642,#9643,
#9644,#9645,#9646,#9647,#9648,#9649,#9650,#9651,#9652,#9653,#9654,#9655,
#9656,#9657,#9658,#9659,#9660,#9661,#9662,#9663,#9664,#9665,#9666,#9667,
#9668,#9669,#9670,#9671,#9672,#9673,#9674,#9675,#9676,#9677,#9678,#9679,
#9680,#9681,#9682,#9683,#9684,#9685,#9686,#9687,#9688,#9689,#9690,#9691,
#9692,#9693,#9694,#9695,#9696,#9697,#9698,#9699,#9700,#9701,#9702,#9703,
#9704,#9705,#9706,#9707,#9708,#9709,#9710,#9711,#9712,#9713,#9714,#9715,
#9716,#9717,#9718,#9719,#9720,#9721,#9722,#9723,#9724,#9725,#9726,#9727,
#9728,#9729,#9730,#9731,#9732),(#9733,#9734,#9735,#9736,#9737,#9738,#9739,
#9740,#9741,#9742,#9743,#9744,#9745,#9746,#9747,#9748,#9749,#9750,#9751,
#9752,#9753,#9754,#9755,#9756,#9757,#9758,#9759,#9760,#9761,#9762,#9763,
#9764,#9765,#9766,#9767,#9768,#9769,#9770,#9771,#9772,#9773,#9774,#9775,
#9776,#9777,#9778,#9779,#9780,#9781,#9782,#9783,#9784,#9785,#9786,#9787,
#9788,#9789,#9790,#9791,#9792,#9793,#9794,#9795,#9796,#9797,#9798,#9799,
#9800,#9801,#9802,#9803,#9804,#9805,#9806,#9807,#9808,#9809,#9810,#9811,
#9812,#9813,#9814,#9815,#9816,#9817,#9818,#9819,#9820,#9821,#9822,#9823,
#9824,#9825,#9826,#9827,#9828,#9829,#9830,#9831,#9832,#9833,#9834,#9835,
#9836,#9837,#9838,#9839,#9840,#9841,#9842,#9843,#9844,#9845,#9846,#9847,
#9848,#9849,#9850,#9851,#9852,#9853,#9854,#9855,#9856,#9857,#9858,#9859,
#9860,#9861,#9862,#9863,#9864,#9865,#9866,#9867,#9868,#9869,#9870,#9871,
#9872,#9873,#9874,#9875,#9876,#9877)),.UNSPECIFIED.,.F.,.F.,.F.)
B_SPLINE_SURFACE_WITH_KNOTS((2,2),(3,2,2,2,2,2,2,2,2,2,2,2,2,2,2,2,2,2,
2,2,2,2,2,2,2,2,2,2,2,2,2,2,2,2,2,2,2,2,2,2,2,2,2,2,2,2,2,2,2,2,2,2,2,2,
2,2,2,2,2,2,2,2,2,2,2,2,2,2,2,2,2,2,3),(0.,1.),(0.,0.0138888888888889,0.0277777777777778,
0.0416666666666667,0.0555555555555556,0.0694444444444444,0.0833333333333333,
0.0972222222222222,0.111111111111111,0.125,0.138888888888889,0.152777777777778,
0.166666666666667,0.180555555555556,0.194444444444444,0.208333333333333,
0.222222222222222,0.236111111111111,0.25,0.263888888888889,0.277777777777778,
0.291666666666667,0.305555555555556,0.319444444444444,0.333333333333333,
0.347222222222222,0.361111111111111,0.375,0.388888888888889,0.402777777777778,
0.416666666666667,0.430555555555556,0.444444444444444,0.458333333333333,
0.472222222222222,0.486111111111111,0.5,0.513888888888889,0.527777777777778,
0.541666666666667,0.555555555555556,0.569444444444444,0.583333333333333,
0.597222222222222,0.611111111111111,0.625,0.638888888888889,0.652777777777778,
0.666666666666667,0.680555555555556,0.694444444444444,0.708333333333333,
0.722222222222222,0.736111111111111,0.75,0.763888888888889,0.777777777777778,
0.791666666666667,0.805555555555556,0.819444444444444,0.833333333333333,
0.847222222222222,0.861111111111111,0.875,0.888888888888889,0.902777777777778,
0.916666666666667,0.930555555555556,0.944444444444444,0.958333333333333,
0.972222222222222,0.986111111111111,1.),.UNSPECIFIED.)
GEOMETRIC_REPRESENTATION_ITEM()
RATIONAL_B_SPLINE_SURFACE(((1.,0.965925826289068,1.,0.965925826289068,1.,
0.965925826289068,1.,0.965925826289068,1.,0.965925826289068,1.,0.965925826289068,
1.,0.965925826289068,1.,0.965925826289068,1.,0.965925826289068,1.,0.965925826289068,
1.,0.965925826289068,1.,0.965925826289068,1.,0.965925826289068,1.,0.965925826289068,
1.,0.965925826289068,1.,0.965925826289068,1.,0.965925826289068,1.,0.965925826289068,
1.,0.965925826289068,1.,0.965925826289068,1.,0.965925826289068,1.,0.965925826289068,
1.,0.965925826289068,1.,0.965925826289068,1.,0.965925826289068,1.,0.965925826289068,
1.,0.965925826289068,1.,0.965925826289068,1.,0.965925826289068,1.,0.965925826289068,
1.,0.965925826289068,1.,0.965925826289068,1.,0.965925826289068,1.,0.965925826289068,
1.,0.965925826289068,1.,0.965925826289068,1.,0.965925826289068,1.,0.965925826289068,
1.,0.965925826289068,1.,0.965925826289068,1.,0.965925826289068,1.,0.965925826289068,
1.,0.965925826289068,1.,0.965925826289068,1.,0.965925826289068,1.,0.965925826289068,
1.,0.965925826289068,1.,0.965925826289068,1.,0.965925826289068,1.,0.965925826289068,
1.,0.965925826289068,1.,0.965925826289068,1.,0.965925826289068,1.,0.965925826289068,
1.,0.965925826289068,1.,0.965925826289068,1.,0.965925826289068,1.,0.965925826289068,
1.,0.965925826289068,1.,0.965925826289068,1.,0.965925826289068,1.,0.965925826289068,
1.,0.965925826289068,1.,0.965925826289068,1.,0.965925826289068,1.,0.965925826289068,
1.,0.965925826289068,1.,0.965925826289068,1.,0.965925826289068,1.,0.965925826289068,
1.,0.965925826289068,1.,0.965925826289068,1.),(1.,0.965925826289068,1.,
0.965925826289068,1.,0.965925826289068,1.,0.965925826289068,1.,0.965925826289068,
1.,0.965925826289068,1.,0.965925826289068,1.,0.965925826289068,1.,0.965925826289068,
1.,0.965925826289068,1.,0.965925826289068,1.,0.965925826289068,1.,0.965925826289068,
1.,0.965925826289068,1.,0.965925826289068,1.,0.965925826289068,1.,0.965925826289068,
1.,0.965925826289068,1.,0.965925826289068,1.,0.965925826289068,1.,0.965925826289068,
1.,0.965925826289068,1.,0.965925826289068,1.,0.965925826289068,1.,0.965925826289068,
1.,0.965925826289068,1.,0.965925826289068,1.,0.965925826289068,1.,0.965925826289068,
1.,0.965925826289068,1.,0.965925826289068,1.,0.965925826289068,1.,0.965925826289068,
1.,0.965925826289068,1.,0.965925826289068,1.,0.965925826289068,1.,0.965925826289068,
1.,0.965925826289068,1.,0.965925826289068,1.,0.965925826289068,1.,0.965925826289068,
1.,0.965925826289068,1.,0.965925826289068,1.,0.965925826289068,1.,0.965925826289068,
1.,0.965925826289068,1.,0.965925826289068,1.,0.965925826289068,1.,0.965925826289068,
1.,0.965925826289068,1.,0.965925826289068,1.,0.965925826289068,1.,0.965925826289068,
1.,0.965925826289068,1.,0.965925826289068,1.,0.965925826289068,1.,0.965925826289068,
1.,0.965925826289068,1.,0.965925826289068,1.,0.965925826289068,1.,0.965925826289068,
1.,0.965925826289068,1.,0.965925826289068,1.,0.965925826289068,1.,0.965925826289068,
1.,0.965925826289068,1.,0.965925826289068,1.,0.965925826289068,1.,0.965925826289068,
1.,0.965925826289068,1.,0.965925826289068,1.,0.965925826289068,1.)))
REPRESENTATION_ITEM('')
SURFACE()
);
#166=(
BOUNDED_SURFACE()
B_SPLINE_SURFACE(1,2,((#9895,#9896,#9897,#9898,#9899,#9900,#9901,#9902,
#9903,#9904,#9905,#9906,#9907,#9908,#9909,#9910,#9911,#9912,#9913,#9914,
#9915,#9916,#9917,#9918,#9919,#9920,#9921,#9922,#9923,#9924,#9925,#9926,
#9927,#9928,#9929,#9930,#9931,#9932,#9933,#9934,#9935,#9936,#9937,#9938,
#9939,#9940,#9941,#9942,#9943,#9944,#9945,#9946,#9947,#9948,#9949,#9950,
#9951,#9952,#9953,#9954,#9955,#9956,#9957,#9958,#9959,#9960,#9961,#9962,
#9963,#9964,#9965,#9966,#9967,#9968,#9969,#9970,#9971,#9972,#9973,#9974,
#9975,#9976,#9977,#9978,#9979,#9980,#9981,#9982,#9983,#9984,#9985,#9986,
#9987,#9988,#9989,#9990,#9991,#9992,#9993,#9994,#9995,#9996,#9997,#9998,
#9999,#10000,#10001,#10002,#10003,#10004,#10005,#10006,#10007,#10008,#10009,
#10010,#10011,#10012,#10013,#10014,#10015,#10016,#10017,#10018,#10019,#10020,
#10021,#10022,#10023,#10024,#10025,#10026,#10027,#10028,#10029,#10030,#10031,
#10032,#10033,#10034,#10035,#10036,#10037,#10038,#10039),(#10040,#10041,
#10042,#10043,#10044,#10045,#10046,#10047,#10048,#10049,#10050,#10051,#10052,
#10053,#10054,#10055,#10056,#10057,#10058,#10059,#10060,#10061,#10062,#10063,
#10064,#10065,#10066,#10067,#10068,#10069,#10070,#10071,#10072,#10073,#10074,
#10075,#10076,#10077,#10078,#10079,#10080,#10081,#10082,#10083,#10084,#10085,
#10086,#10087,#10088,#10089,#10090,#10091,#10092,#10093,#10094,#10095,#10096,
#10097,#10098,#10099,#10100,#10101,#10102,#10103,#10104,#10105,#10106,#10107,
#10108,#10109,#10110,#10111,#10112,#10113,#10114,#10115,#10116,#10117,#10118,
#10119,#10120,#10121,#10122,#10123,#10124,#10125,#10126,#10127,#10128,#10129,
#10130,#10131,#10132,#10133,#10134,#10135,#10136,#10137,#10138,#10139,#10140,
#10141,#10142,#10143,#10144,#10145,#10146,#10147,#10148,#10149,#10150,#10151,
#10152,#10153,#10154,#10155,#10156,#10157,#10158,#10159,#10160,#10161,#10162,
#10163,#10164,#10165,#10166,#10167,#10168,#10169,#10170,#10171,#10172,#10173,
#10174,#10175,#10176,#10177,#10178,#10179,#10180,#10181,#10182,#10183,#10184)),
 .UNSPECIFIED.,.F.,.F.,.F.)
B_SPLINE_SURFACE_WITH_KNOTS((2,2),(3,2,2,2,2,2,2,2,2,2,2,2,2,2,2,2,2,2,
2,2,2,2,2,2,2,2,2,2,2,2,2,2,2,2,2,2,2,2,2,2,2,2,2,2,2,2,2,2,2,2,2,2,2,2,
2,2,2,2,2,2,2,2,2,2,2,2,2,2,2,2,2,2,3),(0.,1.),(0.,0.0138888888888889,0.0277777777777778,
0.0416666666666667,0.0555555555555556,0.0694444444444444,0.0833333333333333,
0.0972222222222222,0.111111111111111,0.125,0.138888888888889,0.152777777777778,
0.166666666666667,0.180555555555556,0.194444444444444,0.208333333333333,
0.222222222222222,0.236111111111111,0.25,0.263888888888889,0.277777777777778,
0.291666666666667,0.305555555555556,0.319444444444444,0.333333333333333,
0.347222222222222,0.361111111111111,0.375,0.388888888888889,0.402777777777778,
0.416666666666667,0.430555555555556,0.444444444444444,0.458333333333333,
0.472222222222222,0.486111111111111,0.5,0.513888888888889,0.527777777777778,
0.541666666666667,0.555555555555556,0.569444444444444,0.583333333333333,
0.597222222222222,0.611111111111111,0.625,0.638888888888889,0.652777777777778,
0.666666666666667,0.680555555555556,0.694444444444444,0.708333333333333,
0.722222222222222,0.736111111111111,0.75,0.763888888888889,0.777777777777778,
0.791666666666667,0.805555555555556,0.819444444444444,0.833333333333333,
0.847222222222222,0.861111111111111,0.875,0.888888888888889,0.902777777777778,
0.916666666666667,0.930555555555556,0.944444444444444,0.958333333333333,
0.972222222222222,0.986111111111111,1.),.UNSPECIFIED.)
GEOMETRIC_REPRESENTATION_ITEM()
RATIONAL_B_SPLINE_SURFACE(((1.,0.965925826289068,1.,0.965925826289068,1.,
0.965925826289068,1.,0.965925826289068,1.,0.965925826289068,1.,0.965925826289068,
1.,0.965925826289068,1.,0.965925826289068,1.,0.965925826289068,1.,0.965925826289068,
1.,0.965925826289068,1.,0.965925826289068,1.,0.965925826289068,1.,0.965925826289068,
1.,0.965925826289068,1.,0.965925826289068,1.,0.965925826289068,1.,0.965925826289068,
1.,0.965925826289068,1.,0.965925826289068,1.,0.965925826289068,1.,0.965925826289068,
1.,0.965925826289068,1.,0.965925826289068,1.,0.965925826289068,1.,0.965925826289068,
1.,0.965925826289068,1.,0.965925826289068,1.,0.965925826289068,1.,0.965925826289068,
1.,0.965925826289068,1.,0.965925826289068,1.,0.965925826289068,1.,0.965925826289068,
1.,0.965925826289068,1.,0.965925826289068,1.,0.965925826289068,1.,0.965925826289068,
1.,0.965925826289068,1.,0.965925826289068,1.,0.965925826289068,1.,0.965925826289068,
1.,0.965925826289068,1.,0.965925826289068,1.,0.965925826289068,1.,0.965925826289068,
1.,0.965925826289068,1.,0.965925826289068,1.,0.965925826289068,1.,0.965925826289068,
1.,0.965925826289068,1.,0.965925826289068,1.,0.965925826289068,1.,0.965925826289068,
1.,0.965925826289068,1.,0.965925826289068,1.,0.965925826289068,1.,0.965925826289068,
1.,0.965925826289068,1.,0.965925826289068,1.,0.965925826289068,1.,0.965925826289068,
1.,0.965925826289068,1.,0.965925826289068,1.,0.965925826289068,1.,0.965925826289068,
1.,0.965925826289068,1.,0.965925826289068,1.,0.965925826289068,1.,0.965925826289068,
1.,0.965925826289068,1.,0.965925826289068,1.),(1.,0.965925826289068,1.,
0.965925826289068,1.,0.965925826289068,1.,0.965925826289068,1.,0.965925826289068,
1.,0.965925826289068,1.,0.965925826289068,1.,0.965925826289068,1.,0.965925826289068,
1.,0.965925826289068,1.,0.965925826289068,1.,0.965925826289068,1.,0.965925826289068,
1.,0.965925826289068,1.,0.965925826289068,1.,0.965925826289068,1.,0.965925826289068,
1.,0.965925826289068,1.,0.965925826289068,1.,0.965925826289068,1.,0.965925826289068,
1.,0.965925826289068,1.,0.965925826289068,1.,0.965925826289068,1.,0.965925826289068,
1.,0.965925826289068,1.,0.965925826289068,1.,0.965925826289068,1.,0.965925826289068,
1.,0.965925826289068,1.,0.965925826289068,1.,0.965925826289068,1.,0.965925826289068,
1.,0.965925826289068,1.,0.965925826289068,1.,0.965925826289068,1.,0.965925826289068,
1.,0.965925826289068,1.,0.965925826289068,1.,0.965925826289068,1.,0.965925826289068,
1.,0.965925826289068,1.,0.965925826289068,1.,0.965925826289068,1.,0.965925826289068,
1.,0.965925826289068,1.,0.965925826289068,1.,0.965925826289068,1.,0.965925826289068,
1.,0.965925826289068,1.,0.965925826289068,1.,0.965925826289068,1.,0.965925826289068,
1.,0.965925826289068,1.,0.965925826289068,1.,0.965925826289068,1.,0.965925826289068,
1.,0.965925826289068,1.,0.965925826289068,1.,0.965925826289068,1.,0.965925826289068,
1.,0.965925826289068,1.,0.965925826289068,1.,0.965925826289068,1.,0.965925826289068,
1.,0.965925826289068,1.,0.965925826289068,1.,0.965925826289068,1.,0.965925826289068,
1.,0.965925826289068,1.,0.965925826289068,1.,0.965925826289068,1.)))
REPRESENTATION_ITEM('')
SURFACE()
);
#167=(
BOUNDED_SURFACE()
B_SPLINE_SURFACE(1,2,((#10210,#10211,#10212,#10213,#10214,#10215,#10216,
#10217,#10218,#10219,#10220,#10221,#10222,#10223,#10224,#10225,#10226,#10227,
#10228,#10229,#10230,#10231,#10232,#10233,#10234,#10235,#10236,#10237,#10238,
#10239,#10240,#10241,#10242,#10243,#10244,#10245,#10246,#10247,#10248,#10249,
#10250,#10251,#10252,#10253,#10254,#10255,#10256,#10257,#10258,#10259,#10260,
#10261,#10262,#10263,#10264,#10265,#10266,#10267,#10268,#10269,#10270,#10271,
#10272,#10273,#10274,#10275,#10276,#10277,#10278,#10279,#10280,#10281,#10282,
#10283,#10284,#10285,#10286,#10287,#10288,#10289,#10290,#10291,#10292,#10293,
#10294,#10295,#10296,#10297,#10298,#10299,#10300,#10301,#10302,#10303,#10304,
#10305,#10306,#10307,#10308,#10309,#10310,#10311,#10312,#10313,#10314,#10315,
#10316,#10317,#10318,#10319,#10320,#10321,#10322,#10323,#10324,#10325,#10326,
#10327,#10328,#10329,#10330,#10331,#10332,#10333,#10334,#10335,#10336,#10337,
#10338,#10339,#10340,#10341,#10342,#10343,#10344,#10345,#10346,#10347,#10348,
#10349,#10350,#10351,#10352,#10353,#10354),(#10355,#10356,#10357,#10358,
#10359,#10360,#10361,#10362,#10363,#10364,#10365,#10366,#10367,#10368,#10369,
#10370,#10371,#10372,#10373,#10374,#10375,#10376,#10377,#10378,#10379,#10380,
#10381,#10382,#10383,#10384,#10385,#10386,#10387,#10388,#10389,#10390,#10391,
#10392,#10393,#10394,#10395,#10396,#10397,#10398,#10399,#10400,#10401,#10402,
#10403,#10404,#10405,#10406,#10407,#10408,#10409,#10410,#10411,#10412,#10413,
#10414,#10415,#10416,#10417,#10418,#10419,#10420,#10421,#10422,#10423,#10424,
#10425,#10426,#10427,#10428,#10429,#10430,#10431,#10432,#10433,#10434,#10435,
#10436,#10437,#10438,#10439,#10440,#10441,#10442,#10443,#10444,#10445,#10446,
#10447,#10448,#10449,#10450,#10451,#10452,#10453,#10454,#10455,#10456,#10457,
#10458,#10459,#10460,#10461,#10462,#10463,#10464,#10465,#10466,#10467,#10468,
#10469,#10470,#10471,#10472,#10473,#10474,#10475,#10476,#10477,#10478,#10479,
#10480,#10481,#10482,#10483,#10484,#10485,#10486,#10487,#10488,#10489,#10490,
#10491,#10492,#10493,#10494,#10495,#10496,#10497,#10498,#10499)),
 .UNSPECIFIED.,.F.,.F.,.F.)
B_SPLINE_SURFACE_WITH_KNOTS((2,2),(3,2,2,2,2,2,2,2,2,2,2,2,2,2,2,2,2,2,
2,2,2,2,2,2,2,2,2,2,2,2,2,2,2,2,2,2,2,2,2,2,2,2,2,2,2,2,2,2,2,2,2,2,2,2,
2,2,2,2,2,2,2,2,2,2,2,2,2,2,2,2,2,2,3),(0.,1.),(0.,0.0138888888888889,0.0277777777777778,
0.0416666666666667,0.0555555555555556,0.0694444444444444,0.0833333333333333,
0.0972222222222222,0.111111111111111,0.125,0.138888888888889,0.152777777777778,
0.166666666666667,0.180555555555556,0.194444444444444,0.208333333333333,
0.222222222222222,0.236111111111111,0.25,0.263888888888889,0.277777777777778,
0.291666666666667,0.305555555555556,0.319444444444444,0.333333333333333,
0.347222222222222,0.361111111111111,0.375,0.388888888888889,0.402777777777778,
0.416666666666667,0.430555555555556,0.444444444444444,0.458333333333333,
0.472222222222222,0.486111111111111,0.5,0.513888888888889,0.527777777777778,
0.541666666666667,0.555555555555556,0.569444444444444,0.583333333333333,
0.597222222222222,0.611111111111111,0.625,0.638888888888889,0.652777777777778,
0.666666666666667,0.680555555555556,0.694444444444444,0.708333333333333,
0.722222222222222,0.736111111111111,0.75,0.763888888888889,0.777777777777778,
0.791666666666667,0.805555555555556,0.819444444444444,0.833333333333333,
0.847222222222222,0.861111111111111,0.875,0.888888888888889,0.902777777777778,
0.916666666666667,0.930555555555556,0.944444444444444,0.958333333333333,
0.972222222222222,0.986111111111111,1.),.UNSPECIFIED.)
GEOMETRIC_REPRESENTATION_ITEM()
RATIONAL_B_SPLINE_SURFACE(((1.,0.965925826289068,1.,0.965925826289068,1.,
0.965925826289068,1.,0.965925826289068,1.,0.965925826289068,1.,0.965925826289068,
1.,0.965925826289068,1.,0.965925826289068,1.,0.965925826289068,1.,0.965925826289068,
1.,0.965925826289068,1.,0.965925826289068,1.,0.965925826289068,1.,0.965925826289068,
1.,0.965925826289068,1.,0.965925826289068,1.,0.965925826289068,1.,0.965925826289068,
1.,0.965925826289068,1.,0.965925826289068,1.,0.965925826289068,1.,0.965925826289068,
1.,0.965925826289068,1.,0.965925826289068,1.,0.965925826289068,1.,0.965925826289068,
1.,0.965925826289068,1.,0.965925826289068,1.,0.965925826289068,1.,0.965925826289068,
1.,0.965925826289068,1.,0.965925826289068,1.,0.965925826289068,1.,0.965925826289068,
1.,0.965925826289068,1.,0.965925826289068,1.,0.965925826289068,1.,0.965925826289068,
1.,0.965925826289068,1.,0.965925826289068,1.,0.965925826289068,1.,0.965925826289068,
1.,0.965925826289068,1.,0.965925826289068,1.,0.965925826289068,1.,0.965925826289068,
1.,0.965925826289068,1.,0.965925826289068,1.,0.965925826289068,1.,0.965925826289068,
1.,0.965925826289068,1.,0.965925826289068,1.,0.965925826289068,1.,0.965925826289068,
1.,0.965925826289068,1.,0.965925826289068,1.,0.965925826289068,1.,0.965925826289068,
1.,0.965925826289068,1.,0.965925826289068,1.,0.965925826289068,1.,0.965925826289068,
1.,0.965925826289068,1.,0.965925826289068,1.,0.965925826289068,1.,0.965925826289068,
1.,0.965925826289068,1.,0.965925826289068,1.,0.965925826289068,1.,0.965925826289068,
1.,0.965925826289068,1.,0.965925826289068,1.),(1.,0.965925826289068,1.,
0.965925826289068,1.,0.965925826289068,1.,0.965925826289068,1.,0.965925826289068,
1.,0.965925826289068,1.,0.965925826289068,1.,0.965925826289068,1.,0.965925826289068,
1.,0.965925826289068,1.,0.965925826289068,1.,0.965925826289068,1.,0.965925826289068,
1.,0.965925826289068,1.,0.965925826289068,1.,0.965925826289068,1.,0.965925826289068,
1.,0.965925826289068,1.,0.965925826289068,1.,0.965925826289068,1.,0.965925826289068,
1.,0.965925826289068,1.,0.965925826289068,1.,0.965925826289068,1.,0.965925826289068,
1.,0.965925826289068,1.,0.965925826289068,1.,0.965925826289068,1.,0.965925826289068,
1.,0.965925826289068,1.,0.965925826289068,1.,0.965925826289068,1.,0.965925826289068,
1.,0.965925826289068,1.,0.965925826289068,1.,0.965925826289068,1.,0.965925826289068,
1.,0.965925826289068,1.,0.965925826289068,1.,0.965925826289068,1.,0.965925826289068,
1.,0.965925826289068,1.,0.965925826289068,1.,0.965925826289068,1.,0.965925826289068,
1.,0.965925826289068,1.,0.965925826289068,1.,0.965925826289068,1.,0.965925826289068,
1.,0.965925826289068,1.,0.965925826289068,1.,0.965925826289068,1.,0.965925826289068,
1.,0.965925826289068,1.,0.965925826289068,1.,0.965925826289068,1.,0.965925826289068,
1.,0.965925826289068,1.,0.965925826289068,1.,0.965925826289068,1.,0.965925826289068,
1.,0.965925826289068,1.,0.965925826289068,1.,0.965925826289068,1.,0.965925826289068,
1.,0.965925826289068,1.,0.965925826289068,1.,0.965925826289068,1.,0.965925826289068,
1.,0.965925826289068,1.,0.965925826289068,1.,0.965925826289068,1.)))
REPRESENTATION_ITEM('')
SURFACE()
);
#168=(
BOUNDED_SURFACE()
B_SPLINE_SURFACE(1,2,((#10531,#10532,#10533,#10534,#10535,#10536,#10537,
#10538,#10539,#10540,#10541,#10542,#10543,#10544,#10545,#10546,#10547,#10548,
#10549,#10550,#10551,#10552,#10553,#10554,#10555,#10556,#10557,#10558,#10559,
#10560,#10561,#10562,#10563,#10564,#10565,#10566,#10567,#10568,#10569,#10570,
#10571,#10572,#10573,#10574,#10575,#10576,#10577,#10578,#10579,#10580,#10581,
#10582,#10583,#10584,#10585,#10586,#10587,#10588,#10589,#10590,#10591,#10592,
#10593,#10594,#10595,#10596,#10597,#10598,#10599,#10600,#10601,#10602,#10603,
#10604,#10605,#10606,#10607,#10608,#10609,#10610,#10611,#10612,#10613,#10614,
#10615,#10616,#10617,#10618,#10619,#10620,#10621,#10622,#10623,#10624,#10625,
#10626,#10627,#10628,#10629,#10630,#10631,#10632,#10633,#10634,#10635,#10636,
#10637,#10638,#10639,#10640,#10641,#10642,#10643,#10644,#10645,#10646,#10647,
#10648,#10649,#10650,#10651,#10652,#10653,#10654,#10655,#10656,#10657,#10658,
#10659,#10660,#10661,#10662,#10663,#10664,#10665,#10666,#10667,#10668,#10669,
#10670,#10671,#10672,#10673,#10674,#10675),(#10676,#10677,#10678,#10679,
#10680,#10681,#10682,#10683,#10684,#10685,#10686,#10687,#10688,#10689,#10690,
#10691,#10692,#10693,#10694,#10695,#10696,#10697,#10698,#10699,#10700,#10701,
#10702,#10703,#10704,#10705,#10706,#10707,#10708,#10709,#10710,#10711,#10712,
#10713,#10714,#10715,#10716,#10717,#10718,#10719,#10720,#10721,#10722,#10723,
#10724,#10725,#10726,#10727,#10728,#10729,#10730,#10731,#10732,#10733,#10734,
#10735,#10736,#10737,#10738,#10739,#10740,#10741,#10742,#10743,#10744,#10745,
#10746,#10747,#10748,#10749,#10750,#10751,#10752,#10753,#10754,#10755,#10756,
#10757,#10758,#10759,#10760,#10761,#10762,#10763,#10764,#10765,#10766,#10767,
#10768,#10769,#10770,#10771,#10772,#10773,#10774,#10775,#10776,#10777,#10778,
#10779,#10780,#10781,#10782,#10783,#10784,#10785,#10786,#10787,#10788,#10789,
#10790,#10791,#10792,#10793,#10794,#10795,#10796,#10797,#10798,#10799,#10800,
#10801,#10802,#10803,#10804,#10805,#10806,#10807,#10808,#10809,#10810,#10811,
#10812,#10813,#10814,#10815,#10816,#10817,#10818,#10819,#10820)),
 .UNSPECIFIED.,.F.,.F.,.F.)
B_SPLINE_SURFACE_WITH_KNOTS((2,2),(3,2,2,2,2,2,2,2,2,2,2,2,2,2,2,2,2,2,
2,2,2,2,2,2,2,2,2,2,2,2,2,2,2,2,2,2,2,2,2,2,2,2,2,2,2,2,2,2,2,2,2,2,2,2,
2,2,2,2,2,2,2,2,2,2,2,2,2,2,2,2,2,2,3),(0.,1.),(0.,0.0138888888888889,0.0277777777777778,
0.0416666666666667,0.0555555555555556,0.0694444444444444,0.0833333333333333,
0.0972222222222222,0.111111111111111,0.125,0.138888888888889,0.152777777777778,
0.166666666666667,0.180555555555556,0.194444444444444,0.208333333333333,
0.222222222222222,0.236111111111111,0.25,0.263888888888889,0.277777777777778,
0.291666666666667,0.305555555555556,0.319444444444444,0.333333333333333,
0.347222222222222,0.361111111111111,0.375,0.388888888888889,0.402777777777778,
0.416666666666667,0.430555555555556,0.444444444444444,0.458333333333333,
0.472222222222222,0.486111111111111,0.5,0.513888888888889,0.527777777777778,
0.541666666666667,0.555555555555556,0.569444444444444,0.583333333333333,
0.597222222222222,0.611111111111111,0.625,0.638888888888889,0.652777777777778,
0.666666666666667,0.680555555555556,0.694444444444444,0.708333333333333,
0.722222222222222,0.736111111111111,0.75,0.763888888888889,0.777777777777778,
0.791666666666667,0.805555555555556,0.819444444444444,0.833333333333333,
0.847222222222222,0.861111111111111,0.875,0.888888888888889,0.902777777777778,
0.916666666666667,0.930555555555556,0.944444444444444,0.958333333333333,
0.972222222222222,0.986111111111111,1.),.UNSPECIFIED.)
GEOMETRIC_REPRESENTATION_ITEM()
RATIONAL_B_SPLINE_SURFACE(((1.,0.965925826289068,1.,0.965925826289068,1.,
0.965925826289068,1.,0.965925826289068,1.,0.965925826289068,1.,0.965925826289068,
1.,0.965925826289068,1.,0.965925826289068,1.,0.965925826289068,1.,0.965925826289068,
1.,0.965925826289068,1.,0.965925826289068,1.,0.965925826289068,1.,0.965925826289068,
1.,0.965925826289068,1.,0.965925826289068,1.,0.965925826289068,1.,0.965925826289068,
1.,0.965925826289068,1.,0.965925826289068,1.,0.965925826289068,1.,0.965925826289068,
1.,0.965925826289068,1.,0.965925826289068,1.,0.965925826289068,1.,0.965925826289068,
1.,0.965925826289068,1.,0.965925826289068,1.,0.965925826289068,1.,0.965925826289068,
1.,0.965925826289068,1.,0.965925826289068,1.,0.965925826289068,1.,0.965925826289068,
1.,0.965925826289068,1.,0.965925826289068,1.,0.965925826289068,1.,0.965925826289068,
1.,0.965925826289068,1.,0.965925826289068,1.,0.965925826289068,1.,0.965925826289068,
1.,0.965925826289068,1.,0.965925826289068,1.,0.965925826289068,1.,0.965925826289068,
1.,0.965925826289068,1.,0.965925826289068,1.,0.965925826289068,1.,0.965925826289068,
1.,0.965925826289068,1.,0.965925826289068,1.,0.965925826289068,1.,0.965925826289068,
1.,0.965925826289068,1.,0.965925826289068,1.,0.965925826289068,1.,0.965925826289068,
1.,0.965925826289068,1.,0.965925826289068,1.,0.965925826289068,1.,0.965925826289068,
1.,0.965925826289068,1.,0.965925826289068,1.,0.965925826289068,1.,0.965925826289068,
1.,0.965925826289068,1.,0.965925826289068,1.,0.965925826289068,1.,0.965925826289068,
1.,0.965925826289068,1.,0.965925826289068,1.),(1.,0.965925826289068,1.,
0.965925826289068,1.,0.965925826289068,1.,0.965925826289068,1.,0.965925826289068,
1.,0.965925826289068,1.,0.965925826289068,1.,0.965925826289068,1.,0.965925826289068,
1.,0.965925826289068,1.,0.965925826289068,1.,0.965925826289068,1.,0.965925826289068,
1.,0.965925826289068,1.,0.965925826289068,1.,0.965925826289068,1.,0.965925826289068,
1.,0.965925826289068,1.,0.965925826289068,1.,0.965925826289068,1.,0.965925826289068,
1.,0.965925826289068,1.,0.965925826289068,1.,0.965925826289068,1.,0.965925826289068,
1.,0.965925826289068,1.,0.965925826289068,1.,0.965925826289068,1.,0.965925826289068,
1.,0.965925826289068,1.,0.965925826289068,1.,0.965925826289068,1.,0.965925826289068,
1.,0.965925826289068,1.,0.965925826289068,1.,0.965925826289068,1.,0.965925826289068,
1.,0.965925826289068,1.,0.965925826289068,1.,0.965925826289068,1.,0.965925826289068,
1.,0.965925826289068,1.,0.965925826289068,1.,0.965925826289068,1.,0.965925826289068,
1.,0.965925826289068,1.,0.965925826289068,1.,0.965925826289068,1.,0.965925826289068,
1.,0.965925826289068,1.,0.965925826289068,1.,0.965925826289068,1.,0.965925826289068,
1.,0.965925826289068,1.,0.965925826289068,1.,0.965925826289068,1.,0.965925826289068,
1.,0.965925826289068,1.,0.965925826289068,1.,0.965925826289068,1.,0.965925826289068,
1.,0.965925826289068,1.,0.965925826289068,1.,0.965925826289068,1.,0.965925826289068,
1.,0.965925826289068,1.,0.965925826289068,1.,0.965925826289068,1.,0.965925826289068,
1.,0.965925826289068,1.,0.965925826289068,1.,0.965925826289068,1.)))
REPRESENTATION_ITEM('')
SURFACE()
);
#169=(
BOUNDED_SURFACE()
B_SPLINE_SURFACE(1,2,((#11117,#11118,#11119,#11120,#11121,#11122,#11123,
#11124,#11125,#11126,#11127,#11128,#11129,#11130,#11131,#11132,#11133,#11134,
#11135,#11136,#11137,#11138,#11139,#11140,#11141,#11142,#11143,#11144,#11145,
#11146,#11147,#11148,#11149,#11150,#11151,#11152,#11153,#11154,#11155,#11156,
#11157,#11158,#11159,#11160,#11161,#11162,#11163,#11164,#11165,#11166,#11167,
#11168,#11169,#11170,#11171,#11172,#11173,#11174,#11175,#11176,#11177,#11178,
#11179,#11180,#11181,#11182,#11183,#11184,#11185,#11186,#11187,#11188,#11189,
#11190,#11191,#11192,#11193,#11194,#11195,#11196,#11197,#11198,#11199,#11200,
#11201,#11202,#11203,#11204,#11205,#11206,#11207,#11208,#11209,#11210,#11211,
#11212,#11213,#11214,#11215,#11216,#11217,#11218,#11219,#11220,#11221,#11222,
#11223,#11224,#11225,#11226,#11227,#11228,#11229,#11230,#11231,#11232,#11233,
#11234,#11235,#11236,#11237,#11238,#11239,#11240,#11241,#11242,#11243,#11244,
#11245,#11246,#11247,#11248,#11249,#11250,#11251,#11252,#11253,#11254,#11255,
#11256,#11257,#11258,#11259,#11260,#11261),(#11262,#11263,#11264,#11265,
#11266,#11267,#11268,#11269,#11270,#11271,#11272,#11273,#11274,#11275,#11276,
#11277,#11278,#11279,#11280,#11281,#11282,#11283,#11284,#11285,#11286,#11287,
#11288,#11289,#11290,#11291,#11292,#11293,#11294,#11295,#11296,#11297,#11298,
#11299,#11300,#11301,#11302,#11303,#11304,#11305,#11306,#11307,#11308,#11309,
#11310,#11311,#11312,#11313,#11314,#11315,#11316,#11317,#11318,#11319,#11320,
#11321,#11322,#11323,#11324,#11325,#11326,#11327,#11328,#11329,#11330,#11331,
#11332,#11333,#11334,#11335,#11336,#11337,#11338,#11339,#11340,#11341,#11342,
#11343,#11344,#11345,#11346,#11347,#11348,#11349,#11350,#11351,#11352,#11353,
#11354,#11355,#11356,#11357,#11358,#11359,#11360,#11361,#11362,#11363,#11364,
#11365,#11366,#11367,#11368,#11369,#11370,#11371,#11372,#11373,#11374,#11375,
#11376,#11377,#11378,#11379,#11380,#11381,#11382,#11383,#11384,#11385,#11386,
#11387,#11388,#11389,#11390,#11391,#11392,#11393,#11394,#11395,#11396,#11397,
#11398,#11399,#11400,#11401,#11402,#11403,#11404,#11405,#11406)),
 .UNSPECIFIED.,.F.,.F.,.F.)
B_SPLINE_SURFACE_WITH_KNOTS((2,2),(3,2,2,2,2,2,2,2,2,2,2,2,2,2,2,2,2,2,
2,2,2,2,2,2,2,2,2,2,2,2,2,2,2,2,2,2,2,2,2,2,2,2,2,2,2,2,2,2,2,2,2,2,2,2,
2,2,2,2,2,2,2,2,2,2,2,2,2,2,2,2,2,2,3),(0.,1.),(0.,0.0138888888888889,0.0277777777777778,
0.0416666666666667,0.0555555555555556,0.0694444444444444,0.0833333333333333,
0.0972222222222222,0.111111111111111,0.125,0.138888888888889,0.152777777777778,
0.166666666666667,0.180555555555556,0.194444444444444,0.208333333333333,
0.222222222222222,0.236111111111111,0.25,0.263888888888889,0.277777777777778,
0.291666666666667,0.305555555555556,0.319444444444444,0.333333333333333,
0.347222222222222,0.361111111111111,0.375,0.388888888888889,0.402777777777778,
0.416666666666667,0.430555555555556,0.444444444444444,0.458333333333333,
0.472222222222222,0.486111111111111,0.5,0.513888888888889,0.527777777777778,
0.541666666666667,0.555555555555556,0.569444444444444,0.583333333333333,
0.597222222222222,0.611111111111111,0.625,0.638888888888889,0.652777777777778,
0.666666666666667,0.680555555555556,0.694444444444444,0.708333333333333,
0.722222222222222,0.736111111111111,0.75,0.763888888888889,0.777777777777778,
0.791666666666667,0.805555555555556,0.819444444444444,0.833333333333333,
0.847222222222222,0.861111111111111,0.875,0.888888888888889,0.902777777777778,
0.916666666666667,0.930555555555556,0.944444444444444,0.958333333333333,
0.972222222222222,0.986111111111111,1.),.UNSPECIFIED.)
GEOMETRIC_REPRESENTATION_ITEM()
RATIONAL_B_SPLINE_SURFACE(((1.,0.965925826289068,1.,0.965925826289068,1.,
0.965925826289068,1.,0.965925826289068,1.,0.965925826289068,1.,0.965925826289068,
1.,0.965925826289068,1.,0.965925826289068,1.,0.965925826289068,1.,0.965925826289068,
1.,0.965925826289068,1.,0.965925826289068,1.,0.965925826289068,1.,0.965925826289068,
1.,0.965925826289068,1.,0.965925826289068,1.,0.965925826289068,1.,0.965925826289068,
1.,0.965925826289068,1.,0.965925826289068,1.,0.965925826289068,1.,0.965925826289068,
1.,0.965925826289068,1.,0.965925826289068,1.,0.965925826289068,1.,0.965925826289068,
1.,0.965925826289068,1.,0.965925826289068,1.,0.965925826289068,1.,0.965925826289068,
1.,0.965925826289068,1.,0.965925826289068,1.,0.965925826289068,1.,0.965925826289068,
1.,0.965925826289068,1.,0.965925826289068,1.,0.965925826289068,1.,0.965925826289068,
1.,0.965925826289068,1.,0.965925826289068,1.,0.965925826289068,1.,0.965925826289068,
1.,0.965925826289068,1.,0.965925826289068,1.,0.965925826289068,1.,0.965925826289068,
1.,0.965925826289068,1.,0.965925826289068,1.,0.965925826289068,1.,0.965925826289068,
1.,0.965925826289068,1.,0.965925826289068,1.,0.965925826289068,1.,0.965925826289068,
1.,0.965925826289068,1.,0.965925826289068,1.,0.965925826289068,1.,0.965925826289068,
1.,0.965925826289068,1.,0.965925826289068,1.,0.965925826289068,1.,0.965925826289068,
1.,0.965925826289068,1.,0.965925826289068,1.,0.965925826289068,1.,0.965925826289068,
1.,0.965925826289068,1.,0.965925826289068,1.,0.965925826289068,1.,0.965925826289068,
1.,0.965925826289068,1.,0.965925826289068,1.),(1.,0.965925826289068,1.,
0.965925826289068,1.,0.965925826289068,1.,0.965925826289068,1.,0.965925826289068,
1.,0.965925826289068,1.,0.965925826289068,1.,0.965925826289068,1.,0.965925826289068,
1.,0.965925826289068,1.,0.965925826289068,1.,0.965925826289068,1.,0.965925826289068,
1.,0.965925826289068,1.,0.965925826289068,1.,0.965925826289068,1.,0.965925826289068,
1.,0.965925826289068,1.,0.965925826289068,1.,0.965925826289068,1.,0.965925826289068,
1.,0.965925826289068,1.,0.965925826289068,1.,0.965925826289068,1.,0.965925826289068,
1.,0.965925826289068,1.,0.965925826289068,1.,0.965925826289068,1.,0.965925826289068,
1.,0.965925826289068,1.,0.965925826289068,1.,0.965925826289068,1.,0.965925826289068,
1.,0.965925826289068,1.,0.965925826289068,1.,0.965925826289068,1.,0.965925826289068,
1.,0.965925826289068,1.,0.965925826289068,1.,0.965925826289068,1.,0.965925826289068,
1.,0.965925826289068,1.,0.965925826289068,1.,0.965925826289068,1.,0.965925826289068,
1.,0.965925826289068,1.,0.965925826289068,1.,0.965925826289068,1.,0.965925826289068,
1.,0.965925826289068,1.,0.965925826289068,1.,0.965925826289068,1.,0.965925826289068,
1.,0.965925826289068,1.,0.965925826289068,1.,0.965925826289068,1.,0.965925826289068,
1.,0.965925826289068,1.,0.965925826289068,1.,0.965925826289068,1.,0.965925826289068,
1.,0.965925826289068,1.,0.965925826289068,1.,0.965925826289068,1.,0.965925826289068,
1.,0.965925826289068,1.,0.965925826289068,1.,0.965925826289068,1.,0.965925826289068,
1.,0.965925826289068,1.,0.965925826289068,1.,0.965925826289068,1.)))
REPRESENTATION_ITEM('')
SURFACE()
);
#170=(
BOUNDED_SURFACE()
B_SPLINE_SURFACE(1,2,((#11430,#11431,#11432,#11433,#11434,#11435,#11436,
#11437,#11438,#11439,#11440,#11441,#11442,#11443,#11444,#11445,#11446,#11447,
#11448,#11449,#11450,#11451,#11452,#11453,#11454,#11455,#11456,#11457,#11458,
#11459,#11460,#11461,#11462,#11463,#11464,#11465,#11466,#11467,#11468,#11469,
#11470,#11471,#11472,#11473,#11474,#11475,#11476,#11477,#11478,#11479,#11480,
#11481,#11482,#11483,#11484,#11485,#11486,#11487,#11488,#11489,#11490,#11491,
#11492,#11493,#11494,#11495,#11496,#11497,#11498,#11499,#11500,#11501,#11502,
#11503,#11504,#11505,#11506,#11507,#11508,#11509,#11510,#11511,#11512,#11513,
#11514,#11515,#11516,#11517,#11518,#11519,#11520,#11521,#11522,#11523,#11524,
#11525,#11526,#11527,#11528,#11529,#11530,#11531,#11532,#11533,#11534,#11535,
#11536,#11537,#11538,#11539,#11540,#11541,#11542,#11543,#11544,#11545,#11546,
#11547,#11548,#11549,#11550,#11551,#11552,#11553,#11554,#11555,#11556,#11557,
#11558,#11559,#11560,#11561,#11562,#11563,#11564,#11565,#11566,#11567,#11568,
#11569,#11570,#11571,#11572,#11573,#11574),(#11575,#11576,#11577,#11578,
#11579,#11580,#11581,#11582,#11583,#11584,#11585,#11586,#11587,#11588,#11589,
#11590,#11591,#11592,#11593,#11594,#11595,#11596,#11597,#11598,#11599,#11600,
#11601,#11602,#11603,#11604,#11605,#11606,#11607,#11608,#11609,#11610,#11611,
#11612,#11613,#11614,#11615,#11616,#11617,#11618,#11619,#11620,#11621,#11622,
#11623,#11624,#11625,#11626,#11627,#11628,#11629,#11630,#11631,#11632,#11633,
#11634,#11635,#11636,#11637,#11638,#11639,#11640,#11641,#11642,#11643,#11644,
#11645,#11646,#11647,#11648,#11649,#11650,#11651,#11652,#11653,#11654,#11655,
#11656,#11657,#11658,#11659,#11660,#11661,#11662,#11663,#11664,#11665,#11666,
#11667,#11668,#11669,#11670,#11671,#11672,#11673,#11674,#11675,#11676,#11677,
#11678,#11679,#11680,#11681,#11682,#11683,#11684,#11685,#11686,#11687,#11688,
#11689,#11690,#11691,#11692,#11693,#11694,#11695,#11696,#11697,#11698,#11699,
#11700,#11701,#11702,#11703,#11704,#11705,#11706,#11707,#11708,#11709,#11710,
#11711,#11712,#11713,#11714,#11715,#11716,#11717,#11718,#11719)),
 .UNSPECIFIED.,.F.,.F.,.F.)
B_SPLINE_SURFACE_WITH_KNOTS((2,2),(3,2,2,2,2,2,2,2,2,2,2,2,2,2,2,2,2,2,
2,2,2,2,2,2,2,2,2,2,2,2,2,2,2,2,2,2,2,2,2,2,2,2,2,2,2,2,2,2,2,2,2,2,2,2,
2,2,2,2,2,2,2,2,2,2,2,2,2,2,2,2,2,2,3),(0.,1.),(0.,0.0138888888888889,0.0277777777777778,
0.0416666666666667,0.0555555555555556,0.0694444444444444,0.0833333333333333,
0.0972222222222222,0.111111111111111,0.125,0.138888888888889,0.152777777777778,
0.166666666666667,0.180555555555556,0.194444444444444,0.208333333333333,
0.222222222222222,0.236111111111111,0.25,0.263888888888889,0.277777777777778,
0.291666666666667,0.305555555555556,0.319444444444444,0.333333333333333,
0.347222222222222,0.361111111111111,0.375,0.388888888888889,0.402777777777778,
0.416666666666667,0.430555555555556,0.444444444444444,0.458333333333333,
0.472222222222222,0.486111111111111,0.5,0.513888888888889,0.527777777777778,
0.541666666666667,0.555555555555556,0.569444444444444,0.583333333333333,
0.597222222222222,0.611111111111111,0.625,0.638888888888889,0.652777777777778,
0.666666666666667,0.680555555555556,0.694444444444444,0.708333333333333,
0.722222222222222,0.736111111111111,0.75,0.763888888888889,0.777777777777778,
0.791666666666667,0.805555555555556,0.819444444444444,0.833333333333333,
0.847222222222222,0.861111111111111,0.875,0.888888888888889,0.902777777777778,
0.916666666666667,0.930555555555556,0.944444444444444,0.958333333333333,
0.972222222222222,0.986111111111111,1.),.UNSPECIFIED.)
GEOMETRIC_REPRESENTATION_ITEM()
RATIONAL_B_SPLINE_SURFACE(((1.,0.965925826289068,1.,0.965925826289068,1.,
0.965925826289068,1.,0.965925826289068,1.,0.965925826289068,1.,0.965925826289068,
1.,0.965925826289068,1.,0.965925826289068,1.,0.965925826289068,1.,0.965925826289068,
1.,0.965925826289068,1.,0.965925826289068,1.,0.965925826289068,1.,0.965925826289068,
1.,0.965925826289068,1.,0.965925826289068,1.,0.965925826289068,1.,0.965925826289068,
1.,0.965925826289068,1.,0.965925826289068,1.,0.965925826289068,1.,0.965925826289068,
1.,0.965925826289068,1.,0.965925826289068,1.,0.965925826289068,1.,0.965925826289068,
1.,0.965925826289068,1.,0.965925826289068,1.,0.965925826289068,1.,0.965925826289068,
1.,0.965925826289068,1.,0.965925826289068,1.,0.965925826289068,1.,0.965925826289068,
1.,0.965925826289068,1.,0.965925826289068,1.,0.965925826289068,1.,0.965925826289068,
1.,0.965925826289068,1.,0.965925826289068,1.,0.965925826289068,1.,0.965925826289068,
1.,0.965925826289068,1.,0.965925826289068,1.,0.965925826289068,1.,0.965925826289068,
1.,0.965925826289068,1.,0.965925826289068,1.,0.965925826289068,1.,0.965925826289068,
1.,0.965925826289068,1.,0.965925826289068,1.,0.965925826289068,1.,0.965925826289068,
1.,0.965925826289068,1.,0.965925826289068,1.,0.965925826289068,1.,0.965925826289068,
1.,0.965925826289068,1.,0.965925826289068,1.,0.965925826289068,1.,0.965925826289068,
1.,0.965925826289068,1.,0.965925826289068,1.,0.965925826289068,1.,0.965925826289068,
1.,0.965925826289068,1.,0.965925826289068,1.,0.965925826289068,1.,0.965925826289068,
1.,0.965925826289068,1.,0.965925826289068,1.),(1.,0.965925826289068,1.,
0.965925826289068,1.,0.965925826289068,1.,0.965925826289068,1.,0.965925826289068,
1.,0.965925826289068,1.,0.965925826289068,1.,0.965925826289068,1.,0.965925826289068,
1.,0.965925826289068,1.,0.965925826289068,1.,0.965925826289068,1.,0.965925826289068,
1.,0.965925826289068,1.,0.965925826289068,1.,0.965925826289068,1.,0.965925826289068,
1.,0.965925826289068,1.,0.965925826289068,1.,0.965925826289068,1.,0.965925826289068,
1.,0.965925826289068,1.,0.965925826289068,1.,0.965925826289068,1.,0.965925826289068,
1.,0.965925826289068,1.,0.965925826289068,1.,0.965925826289068,1.,0.965925826289068,
1.,0.965925826289068,1.,0.965925826289068,1.,0.965925826289068,1.,0.965925826289068,
1.,0.965925826289068,1.,0.965925826289068,1.,0.965925826289068,1.,0.965925826289068,
1.,0.965925826289068,1.,0.965925826289068,1.,0.965925826289068,1.,0.965925826289068,
1.,0.965925826289068,1.,0.965925826289068,1.,0.965925826289068,1.,0.965925826289068,
1.,0.965925826289068,1.,0.965925826289068,1.,0.965925826289068,1.,0.965925826289068,
1.,0.965925826289068,1.,0.965925826289068,1.,0.965925826289068,1.,0.965925826289068,
1.,0.965925826289068,1.,0.965925826289068,1.,0.965925826289068,1.,0.965925826289068,
1.,0.965925826289068,1.,0.965925826289068,1.,0.965925826289068,1.,0.965925826289068,
1.,0.965925826289068,1.,0.965925826289068,1.,0.965925826289068,1.,0.965925826289068,
1.,0.965925826289068,1.,0.965925826289068,1.,0.965925826289068,1.,0.965925826289068,
1.,0.965925826289068,1.,0.965925826289068,1.,0.965925826289068,1.)))
REPRESENTATION_ITEM('')
SURFACE()
);
#171=(
BOUNDED_SURFACE()
B_SPLINE_SURFACE(1,2,((#11750,#11751,#11752,#11753,#11754,#11755,#11756,
#11757,#11758,#11759,#11760,#11761,#11762,#11763,#11764,#11765,#11766,#11767,
#11768,#11769,#11770,#11771,#11772,#11773,#11774,#11775,#11776,#11777,#11778,
#11779,#11780,#11781,#11782,#11783,#11784,#11785,#11786,#11787,#11788,#11789,
#11790,#11791,#11792,#11793,#11794,#11795,#11796,#11797,#11798,#11799,#11800,
#11801,#11802,#11803,#11804,#11805,#11806,#11807,#11808,#11809,#11810,#11811,
#11812,#11813,#11814,#11815,#11816,#11817,#11818,#11819,#11820,#11821,#11822,
#11823,#11824,#11825,#11826,#11827,#11828,#11829,#11830,#11831,#11832,#11833,
#11834,#11835,#11836,#11837,#11838,#11839,#11840,#11841,#11842,#11843,#11844,
#11845,#11846,#11847,#11848,#11849,#11850,#11851,#11852,#11853,#11854,#11855,
#11856,#11857,#11858,#11859,#11860,#11861,#11862,#11863,#11864,#11865,#11866,
#11867,#11868,#11869,#11870,#11871,#11872,#11873,#11874,#11875,#11876,#11877,
#11878,#11879,#11880,#11881,#11882,#11883,#11884,#11885,#11886,#11887,#11888,
#11889,#11890,#11891,#11892,#11893,#11894),(#11895,#11896,#11897,#11898,
#11899,#11900,#11901,#11902,#11903,#11904,#11905,#11906,#11907,#11908,#11909,
#11910,#11911,#11912,#11913,#11914,#11915,#11916,#11917,#11918,#11919,#11920,
#11921,#11922,#11923,#11924,#11925,#11926,#11927,#11928,#11929,#11930,#11931,
#11932,#11933,#11934,#11935,#11936,#11937,#11938,#11939,#11940,#11941,#11942,
#11943,#11944,#11945,#11946,#11947,#11948,#11949,#11950,#11951,#11952,#11953,
#11954,#11955,#11956,#11957,#11958,#11959,#11960,#11961,#11962,#11963,#11964,
#11965,#11966,#11967,#11968,#11969,#11970,#11971,#11972,#11973,#11974,#11975,
#11976,#11977,#11978,#11979,#11980,#11981,#11982,#11983,#11984,#11985,#11986,
#11987,#11988,#11989,#11990,#11991,#11992,#11993,#11994,#11995,#11996,#11997,
#11998,#11999,#12000,#12001,#12002,#12003,#12004,#12005,#12006,#12007,#12008,
#12009,#12010,#12011,#12012,#12013,#12014,#12015,#12016,#12017,#12018,#12019,
#12020,#12021,#12022,#12023,#12024,#12025,#12026,#12027,#12028,#12029,#12030,
#12031,#12032,#12033,#12034,#12035,#12036,#12037,#12038,#12039)),
 .UNSPECIFIED.,.F.,.F.,.F.)
B_SPLINE_SURFACE_WITH_KNOTS((2,2),(3,2,2,2,2,2,2,2,2,2,2,2,2,2,2,2,2,2,
2,2,2,2,2,2,2,2,2,2,2,2,2,2,2,2,2,2,2,2,2,2,2,2,2,2,2,2,2,2,2,2,2,2,2,2,
2,2,2,2,2,2,2,2,2,2,2,2,2,2,2,2,2,2,3),(0.,1.),(0.,0.0138888888888889,0.0277777777777778,
0.0416666666666667,0.0555555555555556,0.0694444444444444,0.0833333333333333,
0.0972222222222222,0.111111111111111,0.125,0.138888888888889,0.152777777777778,
0.166666666666667,0.180555555555556,0.194444444444444,0.208333333333333,
0.222222222222222,0.236111111111111,0.25,0.263888888888889,0.277777777777778,
0.291666666666667,0.305555555555556,0.319444444444444,0.333333333333333,
0.347222222222222,0.361111111111111,0.375,0.388888888888889,0.402777777777778,
0.416666666666667,0.430555555555556,0.444444444444444,0.458333333333333,
0.472222222222222,0.486111111111111,0.5,0.513888888888889,0.527777777777778,
0.541666666666667,0.555555555555556,0.569444444444444,0.583333333333333,
0.597222222222222,0.611111111111111,0.625,0.638888888888889,0.652777777777778,
0.666666666666667,0.680555555555556,0.694444444444444,0.708333333333333,
0.722222222222222,0.736111111111111,0.75,0.763888888888889,0.777777777777778,
0.791666666666667,0.805555555555556,0.819444444444444,0.833333333333333,
0.847222222222222,0.861111111111111,0.875,0.888888888888889,0.902777777777778,
0.916666666666667,0.930555555555556,0.944444444444444,0.958333333333333,
0.972222222222222,0.986111111111111,1.),.UNSPECIFIED.)
GEOMETRIC_REPRESENTATION_ITEM()
RATIONAL_B_SPLINE_SURFACE(((1.,0.965925826289068,1.,0.965925826289068,1.,
0.965925826289068,1.,0.965925826289068,1.,0.965925826289068,1.,0.965925826289068,
1.,0.965925826289068,1.,0.965925826289068,1.,0.965925826289068,1.,0.965925826289068,
1.,0.965925826289068,1.,0.965925826289068,1.,0.965925826289068,1.,0.965925826289068,
1.,0.965925826289068,1.,0.965925826289068,1.,0.965925826289068,1.,0.965925826289068,
1.,0.965925826289068,1.,0.965925826289068,1.,0.965925826289068,1.,0.965925826289068,
1.,0.965925826289068,1.,0.965925826289068,1.,0.965925826289068,1.,0.965925826289068,
1.,0.965925826289068,1.,0.965925826289068,1.,0.965925826289068,1.,0.965925826289068,
1.,0.965925826289068,1.,0.965925826289068,1.,0.965925826289068,1.,0.965925826289068,
1.,0.965925826289068,1.,0.965925826289068,1.,0.965925826289068,1.,0.965925826289068,
1.,0.965925826289068,1.,0.965925826289068,1.,0.965925826289068,1.,0.965925826289068,
1.,0.965925826289068,1.,0.965925826289068,1.,0.965925826289068,1.,0.965925826289068,
1.,0.965925826289068,1.,0.965925826289068,1.,0.965925826289068,1.,0.965925826289068,
1.,0.965925826289068,1.,0.965925826289068,1.,0.965925826289068,1.,0.965925826289068,
1.,0.965925826289068,1.,0.965925826289068,1.,0.965925826289068,1.,0.965925826289068,
1.,0.965925826289068,1.,0.965925826289068,1.,0.965925826289068,1.,0.965925826289068,
1.,0.965925826289068,1.,0.965925826289068,1.,0.965925826289068,1.,0.965925826289068,
1.,0.965925826289068,1.,0.965925826289068,1.,0.965925826289068,1.,0.965925826289068,
1.,0.965925826289068,1.,0.965925826289068,1.),(1.,0.965925826289068,1.,
0.965925826289068,1.,0.965925826289068,1.,0.965925826289068,1.,0.965925826289068,
1.,0.965925826289068,1.,0.965925826289068,1.,0.965925826289068,1.,0.965925826289068,
1.,0.965925826289068,1.,0.965925826289068,1.,0.965925826289068,1.,0.965925826289068,
1.,0.965925826289068,1.,0.965925826289068,1.,0.965925826289068,1.,0.965925826289068,
1.,0.965925826289068,1.,0.965925826289068,1.,0.965925826289068,1.,0.965925826289068,
1.,0.965925826289068,1.,0.965925826289068,1.,0.965925826289068,1.,0.965925826289068,
1.,0.965925826289068,1.,0.965925826289068,1.,0.965925826289068,1.,0.965925826289068,
1.,0.965925826289068,1.,0.965925826289068,1.,0.965925826289068,1.,0.965925826289068,
1.,0.965925826289068,1.,0.965925826289068,1.,0.965925826289068,1.,0.965925826289068,
1.,0.965925826289068,1.,0.965925826289068,1.,0.965925826289068,1.,0.965925826289068,
1.,0.965925826289068,1.,0.965925826289068,1.,0.965925826289068,1.,0.965925826289068,
1.,0.965925826289068,1.,0.965925826289068,1.,0.965925826289068,1.,0.965925826289068,
1.,0.965925826289068,1.,0.965925826289068,1.,0.965925826289068,1.,0.965925826289068,
1.,0.965925826289068,1.,0.965925826289068,1.,0.965925826289068,1.,0.965925826289068,
1.,0.965925826289068,1.,0.965925826289068,1.,0.965925826289068,1.,0.965925826289068,
1.,0.965925826289068,1.,0.965925826289068,1.,0.965925826289068,1.,0.965925826289068,
1.,0.965925826289068,1.,0.965925826289068,1.,0.965925826289068,1.,0.965925826289068,
1.,0.965925826289068,1.,0.965925826289068,1.,0.965925826289068,1.)))
REPRESENTATION_ITEM('')
SURFACE()
);
#172=(
BOUNDED_SURFACE()
B_SPLINE_SURFACE(1,2,((#12056,#12057,#12058,#12059,#12060,#12061,#12062,
#12063,#12064,#12065,#12066,#12067,#12068,#12069,#12070,#12071,#12072,#12073,
#12074,#12075,#12076,#12077,#12078,#12079,#12080,#12081,#12082,#12083,#12084,
#12085,#12086,#12087,#12088,#12089,#12090,#12091,#12092,#12093,#12094,#12095,
#12096,#12097,#12098,#12099,#12100,#12101,#12102,#12103,#12104,#12105,#12106,
#12107,#12108,#12109,#12110,#12111,#12112,#12113,#12114,#12115,#12116,#12117,
#12118,#12119,#12120,#12121,#12122,#12123,#12124,#12125,#12126,#12127,#12128,
#12129,#12130,#12131,#12132,#12133,#12134,#12135,#12136,#12137,#12138,#12139,
#12140,#12141,#12142,#12143,#12144,#12145,#12146,#12147,#12148,#12149,#12150,
#12151,#12152,#12153,#12154,#12155,#12156,#12157,#12158,#12159,#12160,#12161,
#12162,#12163,#12164,#12165,#12166,#12167,#12168,#12169,#12170,#12171,#12172,
#12173,#12174,#12175,#12176,#12177,#12178,#12179,#12180,#12181,#12182,#12183,
#12184,#12185,#12186,#12187,#12188,#12189,#12190,#12191,#12192,#12193,#12194,
#12195,#12196,#12197,#12198,#12199,#12200),(#12201,#12202,#12203,#12204,
#12205,#12206,#12207,#12208,#12209,#12210,#12211,#12212,#12213,#12214,#12215,
#12216,#12217,#12218,#12219,#12220,#12221,#12222,#12223,#12224,#12225,#12226,
#12227,#12228,#12229,#12230,#12231,#12232,#12233,#12234,#12235,#12236,#12237,
#12238,#12239,#12240,#12241,#12242,#12243,#12244,#12245,#12246,#12247,#12248,
#12249,#12250,#12251,#12252,#12253,#12254,#12255,#12256,#12257,#12258,#12259,
#12260,#12261,#12262,#12263,#12264,#12265,#12266,#12267,#12268,#12269,#12270,
#12271,#12272,#12273,#12274,#12275,#12276,#12277,#12278,#12279,#12280,#12281,
#12282,#12283,#12284,#12285,#12286,#12287,#12288,#12289,#12290,#12291,#12292,
#12293,#12294,#12295,#12296,#12297,#12298,#12299,#12300,#12301,#12302,#12303,
#12304,#12305,#12306,#12307,#12308,#12309,#12310,#12311,#12312,#12313,#12314,
#12315,#12316,#12317,#12318,#12319,#12320,#12321,#12322,#12323,#12324,#12325,
#12326,#12327,#12328,#12329,#12330,#12331,#12332,#12333,#12334,#12335,#12336,
#12337,#12338,#12339,#12340,#12341,#12342,#12343,#12344,#12345)),
 .UNSPECIFIED.,.F.,.F.,.F.)
B_SPLINE_SURFACE_WITH_KNOTS((2,2),(3,2,2,2,2,2,2,2,2,2,2,2,2,2,2,2,2,2,
2,2,2,2,2,2,2,2,2,2,2,2,2,2,2,2,2,2,2,2,2,2,2,2,2,2,2,2,2,2,2,2,2,2,2,2,
2,2,2,2,2,2,2,2,2,2,2,2,2,2,2,2,2,2,3),(0.,1.),(0.,0.0138888888888889,0.0277777777777778,
0.0416666666666667,0.0555555555555556,0.0694444444444444,0.0833333333333333,
0.0972222222222222,0.111111111111111,0.125,0.138888888888889,0.152777777777778,
0.166666666666667,0.180555555555556,0.194444444444444,0.208333333333333,
0.222222222222222,0.236111111111111,0.25,0.263888888888889,0.277777777777778,
0.291666666666667,0.305555555555556,0.319444444444444,0.333333333333333,
0.347222222222222,0.361111111111111,0.375,0.388888888888889,0.402777777777778,
0.416666666666667,0.430555555555556,0.444444444444444,0.458333333333333,
0.472222222222222,0.486111111111111,0.5,0.513888888888889,0.527777777777778,
0.541666666666667,0.555555555555556,0.569444444444444,0.583333333333333,
0.597222222222222,0.611111111111111,0.625,0.638888888888889,0.652777777777778,
0.666666666666667,0.680555555555556,0.694444444444444,0.708333333333333,
0.722222222222222,0.736111111111111,0.75,0.763888888888889,0.777777777777778,
0.791666666666667,0.805555555555556,0.819444444444444,0.833333333333333,
0.847222222222222,0.861111111111111,0.875,0.888888888888889,0.902777777777778,
0.916666666666667,0.930555555555556,0.944444444444444,0.958333333333333,
0.972222222222222,0.986111111111111,1.),.UNSPECIFIED.)
GEOMETRIC_REPRESENTATION_ITEM()
RATIONAL_B_SPLINE_SURFACE(((1.,0.965925826289068,1.,0.965925826289068,1.,
0.965925826289068,1.,0.965925826289068,1.,0.965925826289068,1.,0.965925826289068,
1.,0.965925826289068,1.,0.965925826289068,1.,0.965925826289068,1.,0.965925826289068,
1.,0.965925826289068,1.,0.965925826289068,1.,0.965925826289068,1.,0.965925826289068,
1.,0.965925826289068,1.,0.965925826289068,1.,0.965925826289068,1.,0.965925826289068,
1.,0.965925826289068,1.,0.965925826289068,1.,0.965925826289068,1.,0.965925826289068,
1.,0.965925826289068,1.,0.965925826289068,1.,0.965925826289068,1.,0.965925826289068,
1.,0.965925826289068,1.,0.965925826289068,1.,0.965925826289068,1.,0.965925826289068,
1.,0.965925826289068,1.,0.965925826289068,1.,0.965925826289068,1.,0.965925826289068,
1.,0.965925826289068,1.,0.965925826289068,1.,0.965925826289068,1.,0.965925826289068,
1.,0.965925826289068,1.,0.965925826289068,1.,0.965925826289068,1.,0.965925826289068,
1.,0.965925826289068,1.,0.965925826289068,1.,0.965925826289068,1.,0.965925826289068,
1.,0.965925826289068,1.,0.965925826289068,1.,0.965925826289068,1.,0.965925826289068,
1.,0.965925826289068,1.,0.965925826289068,1.,0.965925826289068,1.,0.965925826289068,
1.,0.965925826289068,1.,0.965925826289068,1.,0.965925826289068,1.,0.965925826289068,
1.,0.965925826289068,1.,0.965925826289068,1.,0.965925826289068,1.,0.965925826289068,
1.,0.965925826289068,1.,0.965925826289068,1.,0.965925826289068,1.,0.965925826289068,
1.,0.965925826289068,1.,0.965925826289068,1.,0.965925826289068,1.,0.965925826289068,
1.,0.965925826289068,1.,0.965925826289068,1.),(1.,0.965925826289068,1.,
0.965925826289068,1.,0.965925826289068,1.,0.965925826289068,1.,0.965925826289068,
1.,0.965925826289068,1.,0.965925826289068,1.,0.965925826289068,1.,0.965925826289068,
1.,0.965925826289068,1.,0.965925826289068,1.,0.965925826289068,1.,0.965925826289068,
1.,0.965925826289068,1.,0.965925826289068,1.,0.965925826289068,1.,0.965925826289068,
1.,0.965925826289068,1.,0.965925826289068,1.,0.965925826289068,1.,0.965925826289068,
1.,0.965925826289068,1.,0.965925826289068,1.,0.965925826289068,1.,0.965925826289068,
1.,0.965925826289068,1.,0.965925826289068,1.,0.965925826289068,1.,0.965925826289068,
1.,0.965925826289068,1.,0.965925826289068,1.,0.965925826289068,1.,0.965925826289068,
1.,0.965925826289068,1.,0.965925826289068,1.,0.965925826289068,1.,0.965925826289068,
1.,0.965925826289068,1.,0.965925826289068,1.,0.965925826289068,1.,0.965925826289068,
1.,0.965925826289068,1.,0.965925826289068,1.,0.965925826289068,1.,0.965925826289068,
1.,0.965925826289068,1.,0.965925826289068,1.,0.965925826289068,1.,0.965925826289068,
1.,0.965925826289068,1.,0.965925826289068,1.,0.965925826289068,1.,0.965925826289068,
1.,0.965925826289068,1.,0.965925826289068,1.,0.965925826289068,1.,0.965925826289068,
1.,0.965925826289068,1.,0.965925826289068,1.,0.965925826289068,1.,0.965925826289068,
1.,0.965925826289068,1.,0.965925826289068,1.,0.965925826289068,1.,0.965925826289068,
1.,0.965925826289068,1.,0.965925826289068,1.,0.965925826289068,1.,0.965925826289068,
1.,0.965925826289068,1.,0.965925826289068,1.,0.965925826289068,1.)))
REPRESENTATION_ITEM('')
SURFACE()
);
#173=(
BOUNDED_SURFACE()
B_SPLINE_SURFACE(1,2,((#12362,#12363,#12364,#12365,#12366,#12367,#12368,
#12369,#12370,#12371,#12372,#12373,#12374,#12375,#12376,#12377,#12378,#12379,
#12380,#12381,#12382,#12383,#12384,#12385,#12386,#12387,#12388,#12389,#12390,
#12391,#12392,#12393,#12394,#12395,#12396,#12397,#12398,#12399,#12400,#12401,
#12402,#12403,#12404,#12405,#12406,#12407,#12408,#12409,#12410,#12411,#12412,
#12413,#12414,#12415,#12416,#12417,#12418,#12419,#12420,#12421,#12422,#12423,
#12424,#12425,#12426,#12427,#12428,#12429,#12430,#12431,#12432,#12433,#12434,
#12435,#12436,#12437,#12438,#12439,#12440,#12441,#12442,#12443,#12444,#12445,
#12446,#12447,#12448,#12449,#12450,#12451,#12452,#12453,#12454,#12455,#12456,
#12457,#12458,#12459,#12460,#12461,#12462,#12463,#12464,#12465,#12466,#12467,
#12468,#12469,#12470,#12471,#12472,#12473,#12474,#12475,#12476,#12477,#12478,
#12479,#12480,#12481,#12482,#12483,#12484,#12485,#12486,#12487,#12488,#12489,
#12490,#12491,#12492,#12493,#12494,#12495,#12496,#12497,#12498,#12499,#12500,
#12501,#12502,#12503,#12504,#12505,#12506),(#12507,#12508,#12509,#12510,
#12511,#12512,#12513,#12514,#12515,#12516,#12517,#12518,#12519,#12520,#12521,
#12522,#12523,#12524,#12525,#12526,#12527,#12528,#12529,#12530,#12531,#12532,
#12533,#12534,#12535,#12536,#12537,#12538,#12539,#12540,#12541,#12542,#12543,
#12544,#12545,#12546,#12547,#12548,#12549,#12550,#12551,#12552,#12553,#12554,
#12555,#12556,#12557,#12558,#12559,#12560,#12561,#12562,#12563,#12564,#12565,
#12566,#12567,#12568,#12569,#12570,#12571,#12572,#12573,#12574,#12575,#12576,
#12577,#12578,#12579,#12580,#12581,#12582,#12583,#12584,#12585,#12586,#12587,
#12588,#12589,#12590,#12591,#12592,#12593,#12594,#12595,#12596,#12597,#12598,
#12599,#12600,#12601,#12602,#12603,#12604,#12605,#12606,#12607,#12608,#12609,
#12610,#12611,#12612,#12613,#12614,#12615,#12616,#12617,#12618,#12619,#12620,
#12621,#12622,#12623,#12624,#12625,#12626,#12627,#12628,#12629,#12630,#12631,
#12632,#12633,#12634,#12635,#12636,#12637,#12638,#12639,#12640,#12641,#12642,
#12643,#12644,#12645,#12646,#12647,#12648,#12649,#12650,#12651)),
 .UNSPECIFIED.,.F.,.F.,.F.)
B_SPLINE_SURFACE_WITH_KNOTS((2,2),(3,2,2,2,2,2,2,2,2,2,2,2,2,2,2,2,2,2,
2,2,2,2,2,2,2,2,2,2,2,2,2,2,2,2,2,2,2,2,2,2,2,2,2,2,2,2,2,2,2,2,2,2,2,2,
2,2,2,2,2,2,2,2,2,2,2,2,2,2,2,2,2,2,3),(0.,1.),(0.,0.0138888888888889,0.0277777777777778,
0.0416666666666667,0.0555555555555556,0.0694444444444444,0.0833333333333333,
0.0972222222222222,0.111111111111111,0.125,0.138888888888889,0.152777777777778,
0.166666666666667,0.180555555555556,0.194444444444444,0.208333333333333,
0.222222222222222,0.236111111111111,0.25,0.263888888888889,0.277777777777778,
0.291666666666667,0.305555555555556,0.319444444444444,0.333333333333333,
0.347222222222222,0.361111111111111,0.375,0.388888888888889,0.402777777777778,
0.416666666666667,0.430555555555556,0.444444444444444,0.458333333333333,
0.472222222222222,0.486111111111111,0.5,0.513888888888889,0.527777777777778,
0.541666666666667,0.555555555555556,0.569444444444444,0.583333333333333,
0.597222222222222,0.611111111111111,0.625,0.638888888888889,0.652777777777778,
0.666666666666667,0.680555555555556,0.694444444444444,0.708333333333333,
0.722222222222222,0.736111111111111,0.75,0.763888888888889,0.777777777777778,
0.791666666666667,0.805555555555556,0.819444444444444,0.833333333333333,
0.847222222222222,0.861111111111111,0.875,0.888888888888889,0.902777777777778,
0.916666666666667,0.930555555555556,0.944444444444444,0.958333333333333,
0.972222222222222,0.986111111111111,1.),.UNSPECIFIED.)
GEOMETRIC_REPRESENTATION_ITEM()
RATIONAL_B_SPLINE_SURFACE(((1.,0.965925826289068,1.,0.965925826289068,1.,
0.965925826289068,1.,0.965925826289068,1.,0.965925826289068,1.,0.965925826289068,
1.,0.965925826289068,1.,0.965925826289068,1.,0.965925826289068,1.,0.965925826289068,
1.,0.965925826289068,1.,0.965925826289068,1.,0.965925826289068,1.,0.965925826289068,
1.,0.965925826289068,1.,0.965925826289068,1.,0.965925826289068,1.,0.965925826289068,
1.,0.965925826289068,1.,0.965925826289068,1.,0.965925826289068,1.,0.965925826289068,
1.,0.965925826289068,1.,0.965925826289068,1.,0.965925826289068,1.,0.965925826289068,
1.,0.965925826289068,1.,0.965925826289068,1.,0.965925826289068,1.,0.965925826289068,
1.,0.965925826289068,1.,0.965925826289068,1.,0.965925826289068,1.,0.965925826289068,
1.,0.965925826289068,1.,0.965925826289068,1.,0.965925826289068,1.,0.965925826289068,
1.,0.965925826289068,1.,0.965925826289068,1.,0.965925826289068,1.,0.965925826289068,
1.,0.965925826289068,1.,0.965925826289068,1.,0.965925826289068,1.,0.965925826289068,
1.,0.965925826289068,1.,0.965925826289068,1.,0.965925826289068,1.,0.965925826289068,
1.,0.965925826289068,1.,0.965925826289068,1.,0.965925826289068,1.,0.965925826289068,
1.,0.965925826289068,1.,0.965925826289068,1.,0.965925826289068,1.,0.965925826289068,
1.,0.965925826289068,1.,0.965925826289068,1.,0.965925826289068,1.,0.965925826289068,
1.,0.965925826289068,1.,0.965925826289068,1.,0.965925826289068,1.,0.965925826289068,
1.,0.965925826289068,1.,0.965925826289068,1.,0.965925826289068,1.,0.965925826289068,
1.,0.965925826289068,1.,0.965925826289068,1.),(1.,0.965925826289068,1.,
0.965925826289068,1.,0.965925826289068,1.,0.965925826289068,1.,0.965925826289068,
1.,0.965925826289068,1.,0.965925826289068,1.,0.965925826289068,1.,0.965925826289068,
1.,0.965925826289068,1.,0.965925826289068,1.,0.965925826289068,1.,0.965925826289068,
1.,0.965925826289068,1.,0.965925826289068,1.,0.965925826289068,1.,0.965925826289068,
1.,0.965925826289068,1.,0.965925826289068,1.,0.965925826289068,1.,0.965925826289068,
1.,0.965925826289068,1.,0.965925826289068,1.,0.965925826289068,1.,0.965925826289068,
1.,0.965925826289068,1.,0.965925826289068,1.,0.965925826289068,1.,0.965925826289068,
1.,0.965925826289068,1.,0.965925826289068,1.,0.965925826289068,1.,0.965925826289068,
1.,0.965925826289068,1.,0.965925826289068,1.,0.965925826289068,1.,0.965925826289068,
1.,0.965925826289068,1.,0.965925826289068,1.,0.965925826289068,1.,0.965925826289068,
1.,0.965925826289068,1.,0.965925826289068,1.,0.965925826289068,1.,0.965925826289068,
1.,0.965925826289068,1.,0.965925826289068,1.,0.965925826289068,1.,0.965925826289068,
1.,0.965925826289068,1.,0.965925826289068,1.,0.965925826289068,1.,0.965925826289068,
1.,0.965925826289068,1.,0.965925826289068,1.,0.965925826289068,1.,0.965925826289068,
1.,0.965925826289068,1.,0.965925826289068,1.,0.965925826289068,1.,0.965925826289068,
1.,0.965925826289068,1.,0.965925826289068,1.,0.965925826289068,1.,0.965925826289068,
1.,0.965925826289068,1.,0.965925826289068,1.,0.965925826289068,1.,0.965925826289068,
1.,0.965925826289068,1.,0.965925826289068,1.,0.965925826289068,1.)))
REPRESENTATION_ITEM('')
SURFACE()
);
#174=(
BOUNDED_SURFACE()
B_SPLINE_SURFACE(1,2,((#12668,#12669,#12670,#12671,#12672,#12673,#12674,
#12675,#12676,#12677,#12678,#12679,#12680,#12681,#12682,#12683,#12684,#12685,
#12686,#12687,#12688,#12689,#12690,#12691,#12692,#12693,#12694,#12695,#12696,
#12697,#12698,#12699,#12700,#12701,#12702,#12703,#12704,#12705,#12706,#12707,
#12708,#12709,#12710,#12711,#12712,#12713,#12714,#12715,#12716,#12717,#12718,
#12719,#12720,#12721,#12722,#12723,#12724,#12725,#12726,#12727,#12728,#12729,
#12730,#12731,#12732,#12733,#12734,#12735,#12736,#12737,#12738,#12739,#12740,
#12741,#12742,#12743,#12744,#12745,#12746,#12747,#12748,#12749,#12750,#12751,
#12752,#12753,#12754,#12755,#12756,#12757,#12758,#12759,#12760,#12761,#12762,
#12763,#12764,#12765,#12766,#12767,#12768,#12769,#12770,#12771,#12772,#12773,
#12774,#12775,#12776,#12777,#12778,#12779,#12780,#12781,#12782,#12783,#12784,
#12785,#12786,#12787,#12788,#12789,#12790,#12791,#12792,#12793,#12794,#12795,
#12796,#12797,#12798,#12799,#12800,#12801,#12802,#12803,#12804,#12805,#12806,
#12807,#12808,#12809,#12810,#12811,#12812),(#12813,#12814,#12815,#12816,
#12817,#12818,#12819,#12820,#12821,#12822,#12823,#12824,#12825,#12826,#12827,
#12828,#12829,#12830,#12831,#12832,#12833,#12834,#12835,#12836,#12837,#12838,
#12839,#12840,#12841,#12842,#12843,#12844,#12845,#12846,#12847,#12848,#12849,
#12850,#12851,#12852,#12853,#12854,#12855,#12856,#12857,#12858,#12859,#12860,
#12861,#12862,#12863,#12864,#12865,#12866,#12867,#12868,#12869,#12870,#12871,
#12872,#12873,#12874,#12875,#12876,#12877,#12878,#12879,#12880,#12881,#12882,
#12883,#12884,#12885,#12886,#12887,#12888,#12889,#12890,#12891,#12892,#12893,
#12894,#12895,#12896,#12897,#12898,#12899,#12900,#12901,#12902,#12903,#12904,
#12905,#12906,#12907,#12908,#12909,#12910,#12911,#12912,#12913,#12914,#12915,
#12916,#12917,#12918,#12919,#12920,#12921,#12922,#12923,#12924,#12925,#12926,
#12927,#12928,#12929,#12930,#12931,#12932,#12933,#12934,#12935,#12936,#12937,
#12938,#12939,#12940,#12941,#12942,#12943,#12944,#12945,#12946,#12947,#12948,
#12949,#12950,#12951,#12952,#12953,#12954,#12955,#12956,#12957)),
 .UNSPECIFIED.,.F.,.F.,.F.)
B_SPLINE_SURFACE_WITH_KNOTS((2,2),(3,2,2,2,2,2,2,2,2,2,2,2,2,2,2,2,2,2,
2,2,2,2,2,2,2,2,2,2,2,2,2,2,2,2,2,2,2,2,2,2,2,2,2,2,2,2,2,2,2,2,2,2,2,2,
2,2,2,2,2,2,2,2,2,2,2,2,2,2,2,2,2,2,3),(0.,1.),(0.,0.0138888888888889,0.0277777777777778,
0.0416666666666667,0.0555555555555556,0.0694444444444444,0.0833333333333333,
0.0972222222222222,0.111111111111111,0.125,0.138888888888889,0.152777777777778,
0.166666666666667,0.180555555555556,0.194444444444444,0.208333333333333,
0.222222222222222,0.236111111111111,0.25,0.263888888888889,0.277777777777778,
0.291666666666667,0.305555555555556,0.319444444444444,0.333333333333333,
0.347222222222222,0.361111111111111,0.375,0.388888888888889,0.402777777777778,
0.416666666666667,0.430555555555556,0.444444444444444,0.458333333333333,
0.472222222222222,0.486111111111111,0.5,0.513888888888889,0.527777777777778,
0.541666666666667,0.555555555555556,0.569444444444444,0.583333333333333,
0.597222222222222,0.611111111111111,0.625,0.638888888888889,0.652777777777778,
0.666666666666667,0.680555555555556,0.694444444444444,0.708333333333333,
0.722222222222222,0.736111111111111,0.75,0.763888888888889,0.777777777777778,
0.791666666666667,0.805555555555556,0.819444444444444,0.833333333333333,
0.847222222222222,0.861111111111111,0.875,0.888888888888889,0.902777777777778,
0.916666666666667,0.930555555555556,0.944444444444444,0.958333333333333,
0.972222222222222,0.986111111111111,1.),.UNSPECIFIED.)
GEOMETRIC_REPRESENTATION_ITEM()
RATIONAL_B_SPLINE_SURFACE(((1.,0.965925826289068,1.,0.965925826289068,1.,
0.965925826289068,1.,0.965925826289068,1.,0.965925826289068,1.,0.965925826289068,
1.,0.965925826289068,1.,0.965925826289068,1.,0.965925826289068,1.,0.965925826289068,
1.,0.965925826289068,1.,0.965925826289068,1.,0.965925826289068,1.,0.965925826289068,
1.,0.965925826289068,1.,0.965925826289068,1.,0.965925826289068,1.,0.965925826289068,
1.,0.965925826289068,1.,0.965925826289068,1.,0.965925826289068,1.,0.965925826289068,
1.,0.965925826289068,1.,0.965925826289068,1.,0.965925826289068,1.,0.965925826289068,
1.,0.965925826289068,1.,0.965925826289068,1.,0.965925826289068,1.,0.965925826289068,
1.,0.965925826289068,1.,0.965925826289068,1.,0.965925826289068,1.,0.965925826289068,
1.,0.965925826289068,1.,0.965925826289068,1.,0.965925826289068,1.,0.965925826289068,
1.,0.965925826289068,1.,0.965925826289068,1.,0.965925826289068,1.,0.965925826289068,
1.,0.965925826289068,1.,0.965925826289068,1.,0.965925826289068,1.,0.965925826289068,
1.,0.965925826289068,1.,0.965925826289068,1.,0.965925826289068,1.,0.965925826289068,
1.,0.965925826289068,1.,0.965925826289068,1.,0.965925826289068,1.,0.965925826289068,
1.,0.965925826289068,1.,0.965925826289068,1.,0.965925826289068,1.,0.965925826289068,
1.,0.965925826289068,1.,0.965925826289068,1.,0.965925826289068,1.,0.965925826289068,
1.,0.965925826289068,1.,0.965925826289068,1.,0.965925826289068,1.,0.965925826289068,
1.,0.965925826289068,1.,0.965925826289068,1.,0.965925826289068,1.,0.965925826289068,
1.,0.965925826289068,1.,0.965925826289068,1.),(1.,0.965925826289068,1.,
0.965925826289068,1.,0.965925826289068,1.,0.965925826289068,1.,0.965925826289068,
1.,0.965925826289068,1.,0.965925826289068,1.,0.965925826289068,1.,0.965925826289068,
1.,0.965925826289068,1.,0.965925826289068,1.,0.965925826289068,1.,0.965925826289068,
1.,0.965925826289068,1.,0.965925826289068,1.,0.965925826289068,1.,0.965925826289068,
1.,0.965925826289068,1.,0.965925826289068,1.,0.965925826289068,1.,0.965925826289068,
1.,0.965925826289068,1.,0.965925826289068,1.,0.965925826289068,1.,0.965925826289068,
1.,0.965925826289068,1.,0.965925826289068,1.,0.965925826289068,1.,0.965925826289068,
1.,0.965925826289068,1.,0.965925826289068,1.,0.965925826289068,1.,0.965925826289068,
1.,0.965925826289068,1.,0.965925826289068,1.,0.965925826289068,1.,0.965925826289068,
1.,0.965925826289068,1.,0.965925826289068,1.,0.965925826289068,1.,0.965925826289068,
1.,0.965925826289068,1.,0.965925826289068,1.,0.965925826289068,1.,0.965925826289068,
1.,0.965925826289068,1.,0.965925826289068,1.,0.965925826289068,1.,0.965925826289068,
1.,0.965925826289068,1.,0.965925826289068,1.,0.965925826289068,1.,0.965925826289068,
1.,0.965925826289068,1.,0.965925826289068,1.,0.965925826289068,1.,0.965925826289068,
1.,0.965925826289068,1.,0.965925826289068,1.,0.965925826289068,1.,0.965925826289068,
1.,0.965925826289068,1.,0.965925826289068,1.,0.965925826289068,1.,0.965925826289068,
1.,0.965925826289068,1.,0.965925826289068,1.,0.965925826289068,1.,0.965925826289068,
1.,0.965925826289068,1.,0.965925826289068,1.,0.965925826289068,1.)))
REPRESENTATION_ITEM('')
SURFACE()
);
#175=(
BOUNDED_SURFACE()
B_SPLINE_SURFACE(1,2,((#12974,#12975,#12976,#12977,#12978,#12979,#12980,
#12981,#12982,#12983,#12984,#12985,#12986,#12987,#12988,#12989,#12990,#12991,
#12992,#12993,#12994,#12995,#12996,#12997,#12998,#12999,#13000,#13001,#13002,
#13003,#13004,#13005,#13006,#13007,#13008,#13009,#13010,#13011,#13012,#13013,
#13014,#13015,#13016,#13017,#13018,#13019,#13020,#13021,#13022,#13023,#13024,
#13025,#13026,#13027,#13028,#13029,#13030,#13031,#13032,#13033,#13034,#13035,
#13036,#13037,#13038,#13039,#13040,#13041,#13042,#13043,#13044,#13045,#13046,
#13047,#13048,#13049,#13050,#13051,#13052,#13053,#13054,#13055,#13056,#13057,
#13058,#13059,#13060,#13061,#13062,#13063,#13064,#13065,#13066,#13067,#13068,
#13069,#13070,#13071,#13072,#13073,#13074,#13075,#13076,#13077,#13078,#13079,
#13080,#13081,#13082,#13083,#13084,#13085,#13086,#13087,#13088,#13089,#13090,
#13091,#13092,#13093,#13094,#13095,#13096,#13097,#13098,#13099,#13100,#13101,
#13102,#13103,#13104,#13105,#13106,#13107,#13108,#13109,#13110,#13111,#13112,
#13113,#13114,#13115,#13116,#13117,#13118),(#13119,#13120,#13121,#13122,
#13123,#13124,#13125,#13126,#13127,#13128,#13129,#13130,#13131,#13132,#13133,
#13134,#13135,#13136,#13137,#13138,#13139,#13140,#13141,#13142,#13143,#13144,
#13145,#13146,#13147,#13148,#13149,#13150,#13151,#13152,#13153,#13154,#13155,
#13156,#13157,#13158,#13159,#13160,#13161,#13162,#13163,#13164,#13165,#13166,
#13167,#13168,#13169,#13170,#13171,#13172,#13173,#13174,#13175,#13176,#13177,
#13178,#13179,#13180,#13181,#13182,#13183,#13184,#13185,#13186,#13187,#13188,
#13189,#13190,#13191,#13192,#13193,#13194,#13195,#13196,#13197,#13198,#13199,
#13200,#13201,#13202,#13203,#13204,#13205,#13206,#13207,#13208,#13209,#13210,
#13211,#13212,#13213,#13214,#13215,#13216,#13217,#13218,#13219,#13220,#13221,
#13222,#13223,#13224,#13225,#13226,#13227,#13228,#13229,#13230,#13231,#13232,
#13233,#13234,#13235,#13236,#13237,#13238,#13239,#13240,#13241,#13242,#13243,
#13244,#13245,#13246,#13247,#13248,#13249,#13250,#13251,#13252,#13253,#13254,
#13255,#13256,#13257,#13258,#13259,#13260,#13261,#13262,#13263)),
 .UNSPECIFIED.,.F.,.F.,.F.)
B_SPLINE_SURFACE_WITH_KNOTS((2,2),(3,2,2,2,2,2,2,2,2,2,2,2,2,2,2,2,2,2,
2,2,2,2,2,2,2,2,2,2,2,2,2,2,2,2,2,2,2,2,2,2,2,2,2,2,2,2,2,2,2,2,2,2,2,2,
2,2,2,2,2,2,2,2,2,2,2,2,2,2,2,2,2,2,3),(0.,1.),(0.,0.0138888888888889,0.0277777777777778,
0.0416666666666667,0.0555555555555556,0.0694444444444444,0.0833333333333333,
0.0972222222222222,0.111111111111111,0.125,0.138888888888889,0.152777777777778,
0.166666666666667,0.180555555555556,0.194444444444444,0.208333333333333,
0.222222222222222,0.236111111111111,0.25,0.263888888888889,0.277777777777778,
0.291666666666667,0.305555555555556,0.319444444444444,0.333333333333333,
0.347222222222222,0.361111111111111,0.375,0.388888888888889,0.402777777777778,
0.416666666666667,0.430555555555556,0.444444444444444,0.458333333333333,
0.472222222222222,0.486111111111111,0.5,0.513888888888889,0.527777777777778,
0.541666666666667,0.555555555555556,0.569444444444444,0.583333333333333,
0.597222222222222,0.611111111111111,0.625,0.638888888888889,0.652777777777778,
0.666666666666667,0.680555555555556,0.694444444444444,0.708333333333333,
0.722222222222222,0.736111111111111,0.75,0.763888888888889,0.777777777777778,
0.791666666666667,0.805555555555556,0.819444444444444,0.833333333333333,
0.847222222222222,0.861111111111111,0.875,0.888888888888889,0.902777777777778,
0.916666666666667,0.930555555555556,0.944444444444444,0.958333333333333,
0.972222222222222,0.986111111111111,1.),.UNSPECIFIED.)
GEOMETRIC_REPRESENTATION_ITEM()
RATIONAL_B_SPLINE_SURFACE(((1.,0.965925826289068,1.,0.965925826289068,1.,
0.965925826289068,1.,0.965925826289068,1.,0.965925826289068,1.,0.965925826289068,
1.,0.965925826289068,1.,0.965925826289068,1.,0.965925826289068,1.,0.965925826289068,
1.,0.965925826289068,1.,0.965925826289068,1.,0.965925826289068,1.,0.965925826289068,
1.,0.965925826289068,1.,0.965925826289068,1.,0.965925826289068,1.,0.965925826289068,
1.,0.965925826289068,1.,0.965925826289068,1.,0.965925826289068,1.,0.965925826289068,
1.,0.965925826289068,1.,0.965925826289068,1.,0.965925826289068,1.,0.965925826289068,
1.,0.965925826289068,1.,0.965925826289068,1.,0.965925826289068,1.,0.965925826289068,
1.,0.965925826289068,1.,0.965925826289068,1.,0.965925826289068,1.,0.965925826289068,
1.,0.965925826289068,1.,0.965925826289068,1.,0.965925826289068,1.,0.965925826289068,
1.,0.965925826289068,1.,0.965925826289068,1.,0.965925826289068,1.,0.965925826289068,
1.,0.965925826289068,1.,0.965925826289068,1.,0.965925826289068,1.,0.965925826289068,
1.,0.965925826289068,1.,0.965925826289068,1.,0.965925826289068,1.,0.965925826289068,
1.,0.965925826289068,1.,0.965925826289068,1.,0.965925826289068,1.,0.965925826289068,
1.,0.965925826289068,1.,0.965925826289068,1.,0.965925826289068,1.,0.965925826289068,
1.,0.965925826289068,1.,0.965925826289068,1.,0.965925826289068,1.,0.965925826289068,
1.,0.965925826289068,1.,0.965925826289068,1.,0.965925826289068,1.,0.965925826289068,
1.,0.965925826289068,1.,0.965925826289068,1.,0.965925826289068,1.,0.965925826289068,
1.,0.965925826289068,1.,0.965925826289068,1.),(1.,0.965925826289068,1.,
0.965925826289068,1.,0.965925826289068,1.,0.965925826289068,1.,0.965925826289068,
1.,0.965925826289068,1.,0.965925826289068,1.,0.965925826289068,1.,0.965925826289068,
1.,0.965925826289068,1.,0.965925826289068,1.,0.965925826289068,1.,0.965925826289068,
1.,0.965925826289068,1.,0.965925826289068,1.,0.965925826289068,1.,0.965925826289068,
1.,0.965925826289068,1.,0.965925826289068,1.,0.965925826289068,1.,0.965925826289068,
1.,0.965925826289068,1.,0.965925826289068,1.,0.965925826289068,1.,0.965925826289068,
1.,0.965925826289068,1.,0.965925826289068,1.,0.965925826289068,1.,0.965925826289068,
1.,0.965925826289068,1.,0.965925826289068,1.,0.965925826289068,1.,0.965925826289068,
1.,0.965925826289068,1.,0.965925826289068,1.,0.965925826289068,1.,0.965925826289068,
1.,0.965925826289068,1.,0.965925826289068,1.,0.965925826289068,1.,0.965925826289068,
1.,0.965925826289068,1.,0.965925826289068,1.,0.965925826289068,1.,0.965925826289068,
1.,0.965925826289068,1.,0.965925826289068,1.,0.965925826289068,1.,0.965925826289068,
1.,0.965925826289068,1.,0.965925826289068,1.,0.965925826289068,1.,0.965925826289068,
1.,0.965925826289068,1.,0.965925826289068,1.,0.965925826289068,1.,0.965925826289068,
1.,0.965925826289068,1.,0.965925826289068,1.,0.965925826289068,1.,0.965925826289068,
1.,0.965925826289068,1.,0.965925826289068,1.,0.965925826289068,1.,0.965925826289068,
1.,0.965925826289068,1.,0.965925826289068,1.,0.965925826289068,1.,0.965925826289068,
1.,0.965925826289068,1.,0.965925826289068,1.,0.965925826289068,1.)))
REPRESENTATION_ITEM('')
SURFACE()
);
#176=(
BOUNDED_SURFACE()
B_SPLINE_SURFACE(1,2,((#13280,#13281,#13282,#13283,#13284,#13285,#13286,
#13287,#13288,#13289,#13290,#13291,#13292,#13293,#13294,#13295,#13296,#13297,
#13298,#13299,#13300,#13301,#13302,#13303,#13304,#13305,#13306,#13307,#13308,
#13309,#13310,#13311,#13312,#13313,#13314,#13315,#13316,#13317,#13318,#13319,
#13320,#13321,#13322,#13323,#13324,#13325,#13326,#13327,#13328,#13329,#13330,
#13331,#13332,#13333,#13334,#13335,#13336,#13337,#13338,#13339,#13340,#13341,
#13342,#13343,#13344,#13345,#13346,#13347,#13348,#13349,#13350,#13351,#13352,
#13353,#13354,#13355,#13356,#13357,#13358,#13359,#13360,#13361,#13362,#13363,
#13364,#13365,#13366,#13367,#13368,#13369,#13370,#13371,#13372,#13373,#13374,
#13375,#13376,#13377,#13378,#13379,#13380,#13381,#13382,#13383,#13384,#13385,
#13386,#13387,#13388,#13389,#13390,#13391,#13392,#13393,#13394,#13395,#13396,
#13397,#13398,#13399,#13400,#13401,#13402,#13403,#13404,#13405,#13406,#13407,
#13408,#13409,#13410,#13411,#13412,#13413,#13414,#13415,#13416,#13417,#13418,
#13419,#13420,#13421,#13422,#13423,#13424),(#13425,#13426,#13427,#13428,
#13429,#13430,#13431,#13432,#13433,#13434,#13435,#13436,#13437,#13438,#13439,
#13440,#13441,#13442,#13443,#13444,#13445,#13446,#13447,#13448,#13449,#13450,
#13451,#13452,#13453,#13454,#13455,#13456,#13457,#13458,#13459,#13460,#13461,
#13462,#13463,#13464,#13465,#13466,#13467,#13468,#13469,#13470,#13471,#13472,
#13473,#13474,#13475,#13476,#13477,#13478,#13479,#13480,#13481,#13482,#13483,
#13484,#13485,#13486,#13487,#13488,#13489,#13490,#13491,#13492,#13493,#13494,
#13495,#13496,#13497,#13498,#13499,#13500,#13501,#13502,#13503,#13504,#13505,
#13506,#13507,#13508,#13509,#13510,#13511,#13512,#13513,#13514,#13515,#13516,
#13517,#13518,#13519,#13520,#13521,#13522,#13523,#13524,#13525,#13526,#13527,
#13528,#13529,#13530,#13531,#13532,#13533,#13534,#13535,#13536,#13537,#13538,
#13539,#13540,#13541,#13542,#13543,#13544,#13545,#13546,#13547,#13548,#13549,
#13550,#13551,#13552,#13553,#13554,#13555,#13556,#13557,#13558,#13559,#13560,
#13561,#13562,#13563,#13564,#13565,#13566,#13567,#13568,#13569)),
 .UNSPECIFIED.,.F.,.F.,.F.)
B_SPLINE_SURFACE_WITH_KNOTS((2,2),(3,2,2,2,2,2,2,2,2,2,2,2,2,2,2,2,2,2,
2,2,2,2,2,2,2,2,2,2,2,2,2,2,2,2,2,2,2,2,2,2,2,2,2,2,2,2,2,2,2,2,2,2,2,2,
2,2,2,2,2,2,2,2,2,2,2,2,2,2,2,2,2,2,3),(0.,1.),(0.,0.0138888888888889,0.0277777777777778,
0.0416666666666667,0.0555555555555556,0.0694444444444444,0.0833333333333333,
0.0972222222222222,0.111111111111111,0.125,0.138888888888889,0.152777777777778,
0.166666666666667,0.180555555555556,0.194444444444444,0.208333333333333,
0.222222222222222,0.236111111111111,0.25,0.263888888888889,0.277777777777778,
0.291666666666667,0.305555555555556,0.319444444444444,0.333333333333333,
0.347222222222222,0.361111111111111,0.375,0.388888888888889,0.402777777777778,
0.416666666666667,0.430555555555556,0.444444444444444,0.458333333333333,
0.472222222222222,0.486111111111111,0.5,0.513888888888889,0.527777777777778,
0.541666666666667,0.555555555555556,0.569444444444444,0.583333333333333,
0.597222222222222,0.611111111111111,0.625,0.638888888888889,0.652777777777778,
0.666666666666667,0.680555555555556,0.694444444444444,0.708333333333333,
0.722222222222222,0.736111111111111,0.75,0.763888888888889,0.777777777777778,
0.791666666666667,0.805555555555556,0.819444444444444,0.833333333333333,
0.847222222222222,0.861111111111111,0.875,0.888888888888889,0.902777777777778,
0.916666666666667,0.930555555555556,0.944444444444444,0.958333333333333,
0.972222222222222,0.986111111111111,1.),.UNSPECIFIED.)
GEOMETRIC_REPRESENTATION_ITEM()
RATIONAL_B_SPLINE_SURFACE(((1.,0.965925826289068,1.,0.965925826289068,1.,
0.965925826289068,1.,0.965925826289068,1.,0.965925826289068,1.,0.965925826289068,
1.,0.965925826289068,1.,0.965925826289068,1.,0.965925826289068,1.,0.965925826289068,
1.,0.965925826289068,1.,0.965925826289068,1.,0.965925826289068,1.,0.965925826289068,
1.,0.965925826289068,1.,0.965925826289068,1.,0.965925826289068,1.,0.965925826289068,
1.,0.965925826289068,1.,0.965925826289068,1.,0.965925826289068,1.,0.965925826289068,
1.,0.965925826289068,1.,0.965925826289068,1.,0.965925826289068,1.,0.965925826289068,
1.,0.965925826289068,1.,0.965925826289068,1.,0.965925826289068,1.,0.965925826289068,
1.,0.965925826289068,1.,0.965925826289068,1.,0.965925826289068,1.,0.965925826289068,
1.,0.965925826289068,1.,0.965925826289068,1.,0.965925826289068,1.,0.965925826289068,
1.,0.965925826289068,1.,0.965925826289068,1.,0.965925826289068,1.,0.965925826289068,
1.,0.965925826289068,1.,0.965925826289068,1.,0.965925826289068,1.,0.965925826289068,
1.,0.965925826289068,1.,0.965925826289068,1.,0.965925826289068,1.,0.965925826289068,
1.,0.965925826289068,1.,0.965925826289068,1.,0.965925826289068,1.,0.965925826289068,
1.,0.965925826289068,1.,0.965925826289068,1.,0.965925826289068,1.,0.965925826289068,
1.,0.965925826289068,1.,0.965925826289068,1.,0.965925826289068,1.,0.965925826289068,
1.,0.965925826289068,1.,0.965925826289068,1.,0.965925826289068,1.,0.965925826289068,
1.,0.965925826289068,1.,0.965925826289068,1.,0.965925826289068,1.,0.965925826289068,
1.,0.965925826289068,1.,0.965925826289068,1.),(1.,0.965925826289068,1.,
0.965925826289068,1.,0.965925826289068,1.,0.965925826289068,1.,0.965925826289068,
1.,0.965925826289068,1.,0.965925826289068,1.,0.965925826289068,1.,0.965925826289068,
1.,0.965925826289068,1.,0.965925826289068,1.,0.965925826289068,1.,0.965925826289068,
1.,0.965925826289068,1.,0.965925826289068,1.,0.965925826289068,1.,0.965925826289068,
1.,0.965925826289068,1.,0.965925826289068,1.,0.965925826289068,1.,0.965925826289068,
1.,0.965925826289068,1.,0.965925826289068,1.,0.965925826289068,1.,0.965925826289068,
1.,0.965925826289068,1.,0.965925826289068,1.,0.965925826289068,1.,0.965925826289068,
1.,0.965925826289068,1.,0.965925826289068,1.,0.965925826289068,1.,0.965925826289068,
1.,0.965925826289068,1.,0.965925826289068,1.,0.965925826289068,1.,0.965925826289068,
1.,0.965925826289068,1.,0.965925826289068,1.,0.965925826289068,1.,0.965925826289068,
1.,0.965925826289068,1.,0.965925826289068,1.,0.965925826289068,1.,0.965925826289068,
1.,0.965925826289068,1.,0.965925826289068,1.,0.965925826289068,1.,0.965925826289068,
1.,0.965925826289068,1.,0.965925826289068,1.,0.965925826289068,1.,0.965925826289068,
1.,0.965925826289068,1.,0.965925826289068,1.,0.965925826289068,1.,0.965925826289068,
1.,0.965925826289068,1.,0.965925826289068,1.,0.965925826289068,1.,0.965925826289068,
1.,0.965925826289068,1.,0.965925826289068,1.,0.965925826289068,1.,0.965925826289068,
1.,0.965925826289068,1.,0.965925826289068,1.,0.965925826289068,1.,0.965925826289068,
1.,0.965925826289068,1.,0.965925826289068,1.,0.965925826289068,1.)))
REPRESENTATION_ITEM('')
SURFACE()
);
#177=(
BOUNDED_SURFACE()
B_SPLINE_SURFACE(1,2,((#13586,#13587,#13588,#13589,#13590,#13591,#13592,
#13593,#13594,#13595,#13596,#13597,#13598,#13599,#13600,#13601,#13602,#13603,
#13604,#13605,#13606,#13607,#13608,#13609,#13610,#13611,#13612,#13613,#13614,
#13615,#13616,#13617,#13618,#13619,#13620,#13621,#13622,#13623,#13624,#13625,
#13626,#13627,#13628,#13629,#13630,#13631,#13632,#13633,#13634,#13635,#13636,
#13637,#13638,#13639,#13640,#13641,#13642,#13643,#13644,#13645,#13646,#13647,
#13648,#13649,#13650,#13651,#13652,#13653,#13654,#13655,#13656,#13657,#13658,
#13659,#13660,#13661,#13662,#13663,#13664,#13665,#13666,#13667,#13668,#13669,
#13670,#13671,#13672,#13673,#13674,#13675,#13676,#13677,#13678,#13679,#13680,
#13681,#13682,#13683,#13684,#13685,#13686,#13687,#13688,#13689,#13690,#13691,
#13692,#13693,#13694,#13695,#13696,#13697,#13698,#13699,#13700,#13701,#13702,
#13703,#13704,#13705,#13706,#13707,#13708,#13709,#13710,#13711,#13712,#13713,
#13714,#13715,#13716,#13717,#13718,#13719,#13720,#13721,#13722,#13723,#13724,
#13725,#13726,#13727,#13728,#13729,#13730),(#13731,#13732,#13733,#13734,
#13735,#13736,#13737,#13738,#13739,#13740,#13741,#13742,#13743,#13744,#13745,
#13746,#13747,#13748,#13749,#13750,#13751,#13752,#13753,#13754,#13755,#13756,
#13757,#13758,#13759,#13760,#13761,#13762,#13763,#13764,#13765,#13766,#13767,
#13768,#13769,#13770,#13771,#13772,#13773,#13774,#13775,#13776,#13777,#13778,
#13779,#13780,#13781,#13782,#13783,#13784,#13785,#13786,#13787,#13788,#13789,
#13790,#13791,#13792,#13793,#13794,#13795,#13796,#13797,#13798,#13799,#13800,
#13801,#13802,#13803,#13804,#13805,#13806,#13807,#13808,#13809,#13810,#13811,
#13812,#13813,#13814,#13815,#13816,#13817,#13818,#13819,#13820,#13821,#13822,
#13823,#13824,#13825,#13826,#13827,#13828,#13829,#13830,#13831,#13832,#13833,
#13834,#13835,#13836,#13837,#13838,#13839,#13840,#13841,#13842,#13843,#13844,
#13845,#13846,#13847,#13848,#13849,#13850,#13851,#13852,#13853,#13854,#13855,
#13856,#13857,#13858,#13859,#13860,#13861,#13862,#13863,#13864,#13865,#13866,
#13867,#13868,#13869,#13870,#13871,#13872,#13873,#13874,#13875)),
 .UNSPECIFIED.,.F.,.F.,.F.)
B_SPLINE_SURFACE_WITH_KNOTS((2,2),(3,2,2,2,2,2,2,2,2,2,2,2,2,2,2,2,2,2,
2,2,2,2,2,2,2,2,2,2,2,2,2,2,2,2,2,2,2,2,2,2,2,2,2,2,2,2,2,2,2,2,2,2,2,2,
2,2,2,2,2,2,2,2,2,2,2,2,2,2,2,2,2,2,3),(0.,1.),(0.,0.0138888888888889,0.0277777777777778,
0.0416666666666667,0.0555555555555556,0.0694444444444444,0.0833333333333333,
0.0972222222222222,0.111111111111111,0.125,0.138888888888889,0.152777777777778,
0.166666666666667,0.180555555555556,0.194444444444444,0.208333333333333,
0.222222222222222,0.236111111111111,0.25,0.263888888888889,0.277777777777778,
0.291666666666667,0.305555555555556,0.319444444444444,0.333333333333333,
0.347222222222222,0.361111111111111,0.375,0.388888888888889,0.402777777777778,
0.416666666666667,0.430555555555556,0.444444444444444,0.458333333333333,
0.472222222222222,0.486111111111111,0.5,0.513888888888889,0.527777777777778,
0.541666666666667,0.555555555555556,0.569444444444444,0.583333333333333,
0.597222222222222,0.611111111111111,0.625,0.638888888888889,0.652777777777778,
0.666666666666667,0.680555555555556,0.694444444444444,0.708333333333333,
0.722222222222222,0.736111111111111,0.75,0.763888888888889,0.777777777777778,
0.791666666666667,0.805555555555556,0.819444444444444,0.833333333333333,
0.847222222222222,0.861111111111111,0.875,0.888888888888889,0.902777777777778,
0.916666666666667,0.930555555555556,0.944444444444444,0.958333333333333,
0.972222222222222,0.986111111111111,1.),.UNSPECIFIED.)
GEOMETRIC_REPRESENTATION_ITEM()
RATIONAL_B_SPLINE_SURFACE(((1.,0.965925826289068,1.,0.965925826289068,1.,
0.965925826289068,1.,0.965925826289068,1.,0.965925826289068,1.,0.965925826289068,
1.,0.965925826289068,1.,0.965925826289068,1.,0.965925826289068,1.,0.965925826289068,
1.,0.965925826289068,1.,0.965925826289068,1.,0.965925826289068,1.,0.965925826289068,
1.,0.965925826289068,1.,0.965925826289068,1.,0.965925826289068,1.,0.965925826289068,
1.,0.965925826289068,1.,0.965925826289068,1.,0.965925826289068,1.,0.965925826289068,
1.,0.965925826289068,1.,0.965925826289068,1.,0.965925826289068,1.,0.965925826289068,
1.,0.965925826289068,1.,0.965925826289068,1.,0.965925826289068,1.,0.965925826289068,
1.,0.965925826289068,1.,0.965925826289068,1.,0.965925826289068,1.,0.965925826289068,
1.,0.965925826289068,1.,0.965925826289068,1.,0.965925826289068,1.,0.965925826289068,
1.,0.965925826289068,1.,0.965925826289068,1.,0.965925826289068,1.,0.965925826289068,
1.,0.965925826289068,1.,0.965925826289068,1.,0.965925826289068,1.,0.965925826289068,
1.,0.965925826289068,1.,0.965925826289068,1.,0.965925826289068,1.,0.965925826289068,
1.,0.965925826289068,1.,0.965925826289068,1.,0.965925826289068,1.,0.965925826289068,
1.,0.965925826289068,1.,0.965925826289068,1.,0.965925826289068,1.,0.965925826289068,
1.,0.965925826289068,1.,0.965925826289068,1.,0.965925826289068,1.,0.965925826289068,
1.,0.965925826289068,1.,0.965925826289068,1.,0.965925826289068,1.,0.965925826289068,
1.,0.965925826289068,1.,0.965925826289068,1.,0.965925826289068,1.,0.965925826289068,
1.,0.965925826289068,1.,0.965925826289068,1.),(1.,0.965925826289068,1.,
0.965925826289068,1.,0.965925826289068,1.,0.965925826289068,1.,0.965925826289068,
1.,0.965925826289068,1.,0.965925826289068,1.,0.965925826289068,1.,0.965925826289068,
1.,0.965925826289068,1.,0.965925826289068,1.,0.965925826289068,1.,0.965925826289068,
1.,0.965925826289068,1.,0.965925826289068,1.,0.965925826289068,1.,0.965925826289068,
1.,0.965925826289068,1.,0.965925826289068,1.,0.965925826289068,1.,0.965925826289068,
1.,0.965925826289068,1.,0.965925826289068,1.,0.965925826289068,1.,0.965925826289068,
1.,0.965925826289068,1.,0.965925826289068,1.,0.965925826289068,1.,0.965925826289068,
1.,0.965925826289068,1.,0.965925826289068,1.,0.965925826289068,1.,0.965925826289068,
1.,0.965925826289068,1.,0.965925826289068,1.,0.965925826289068,1.,0.965925826289068,
1.,0.965925826289068,1.,0.965925826289068,1.,0.965925826289068,1.,0.965925826289068,
1.,0.965925826289068,1.,0.965925826289068,1.,0.965925826289068,1.,0.965925826289068,
1.,0.965925826289068,1.,0.965925826289068,1.,0.965925826289068,1.,0.965925826289068,
1.,0.965925826289068,1.,0.965925826289068,1.,0.965925826289068,1.,0.965925826289068,
1.,0.965925826289068,1.,0.965925826289068,1.,0.965925826289068,1.,0.965925826289068,
1.,0.965925826289068,1.,0.965925826289068,1.,0.965925826289068,1.,0.965925826289068,
1.,0.965925826289068,1.,0.965925826289068,1.,0.965925826289068,1.,0.965925826289068,
1.,0.965925826289068,1.,0.965925826289068,1.,0.965925826289068,1.,0.965925826289068,
1.,0.965925826289068,1.,0.965925826289068,1.,0.965925826289068,1.)))
REPRESENTATION_ITEM('')
SURFACE()
);
#178=(
BOUNDED_SURFACE()
B_SPLINE_SURFACE(1,2,((#13887,#13888,#13889,#13890,#13891,#13892,#13893,
#13894,#13895,#13896,#13897,#13898,#13899,#13900,#13901,#13902,#13903,#13904,
#13905,#13906,#13907,#13908,#13909,#13910,#13911,#13912,#13913,#13914,#13915,
#13916,#13917,#13918,#13919,#13920,#13921,#13922,#13923,#13924,#13925,#13926,
#13927,#13928,#13929,#13930,#13931,#13932,#13933,#13934,#13935,#13936,#13937,
#13938,#13939,#13940,#13941,#13942,#13943,#13944,#13945,#13946,#13947,#13948,
#13949,#13950,#13951,#13952,#13953,#13954,#13955,#13956,#13957,#13958,#13959,
#13960,#13961,#13962,#13963,#13964,#13965,#13966,#13967,#13968,#13969,#13970,
#13971,#13972,#13973,#13974,#13975,#13976,#13977,#13978,#13979,#13980,#13981,
#13982,#13983,#13984,#13985,#13986,#13987,#13988,#13989,#13990,#13991,#13992,
#13993,#13994,#13995,#13996,#13997,#13998,#13999,#14000,#14001,#14002,#14003,
#14004,#14005,#14006,#14007,#14008,#14009,#14010,#14011,#14012,#14013,#14014,
#14015,#14016,#14017,#14018,#14019,#14020,#14021,#14022,#14023,#14024,#14025,
#14026,#14027,#14028,#14029,#14030,#14031),(#14032,#14033,#14034,#14035,
#14036,#14037,#14038,#14039,#14040,#14041,#14042,#14043,#14044,#14045,#14046,
#14047,#14048,#14049,#14050,#14051,#14052,#14053,#14054,#14055,#14056,#14057,
#14058,#14059,#14060,#14061,#14062,#14063,#14064,#14065,#14066,#14067,#14068,
#14069,#14070,#14071,#14072,#14073,#14074,#14075,#14076,#14077,#14078,#14079,
#14080,#14081,#14082,#14083,#14084,#14085,#14086,#14087,#14088,#14089,#14090,
#14091,#14092,#14093,#14094,#14095,#14096,#14097,#14098,#14099,#14100,#14101,
#14102,#14103,#14104,#14105,#14106,#14107,#14108,#14109,#14110,#14111,#14112,
#14113,#14114,#14115,#14116,#14117,#14118,#14119,#14120,#14121,#14122,#14123,
#14124,#14125,#14126,#14127,#14128,#14129,#14130,#14131,#14132,#14133,#14134,
#14135,#14136,#14137,#14138,#14139,#14140,#14141,#14142,#14143,#14144,#14145,
#14146,#14147,#14148,#14149,#14150,#14151,#14152,#14153,#14154,#14155,#14156,
#14157,#14158,#14159,#14160,#14161,#14162,#14163,#14164,#14165,#14166,#14167,
#14168,#14169,#14170,#14171,#14172,#14173,#14174,#14175,#14176)),
 .UNSPECIFIED.,.F.,.F.,.F.)
B_SPLINE_SURFACE_WITH_KNOTS((2,2),(3,2,2,2,2,2,2,2,2,2,2,2,2,2,2,2,2,2,
2,2,2,2,2,2,2,2,2,2,2,2,2,2,2,2,2,2,2,2,2,2,2,2,2,2,2,2,2,2,2,2,2,2,2,2,
2,2,2,2,2,2,2,2,2,2,2,2,2,2,2,2,2,2,3),(0.,1.),(0.,0.0138888888888889,0.0277777777777778,
0.0416666666666667,0.0555555555555556,0.0694444444444444,0.0833333333333333,
0.0972222222222222,0.111111111111111,0.125,0.138888888888889,0.152777777777778,
0.166666666666667,0.180555555555556,0.194444444444444,0.208333333333333,
0.222222222222222,0.236111111111111,0.25,0.263888888888889,0.277777777777778,
0.291666666666667,0.305555555555556,0.319444444444444,0.333333333333333,
0.347222222222222,0.361111111111111,0.375,0.388888888888889,0.402777777777778,
0.416666666666667,0.430555555555556,0.444444444444444,0.458333333333333,
0.472222222222222,0.486111111111111,0.5,0.513888888888889,0.527777777777778,
0.541666666666667,0.555555555555556,0.569444444444444,0.583333333333333,
0.597222222222222,0.611111111111111,0.625,0.638888888888889,0.652777777777778,
0.666666666666667,0.680555555555556,0.694444444444444,0.708333333333333,
0.722222222222222,0.736111111111111,0.75,0.763888888888889,0.777777777777778,
0.791666666666667,0.805555555555556,0.819444444444444,0.833333333333333,
0.847222222222222,0.861111111111111,0.875,0.888888888888889,0.902777777777778,
0.916666666666667,0.930555555555556,0.944444444444444,0.958333333333333,
0.972222222222222,0.986111111111111,1.),.UNSPECIFIED.)
GEOMETRIC_REPRESENTATION_ITEM()
RATIONAL_B_SPLINE_SURFACE(((1.,0.965925826289068,1.,0.965925826289068,1.,
0.965925826289068,1.,0.965925826289068,1.,0.965925826289068,1.,0.965925826289068,
1.,0.965925826289068,1.,0.965925826289068,1.,0.965925826289068,1.,0.965925826289068,
1.,0.965925826289068,1.,0.965925826289068,1.,0.965925826289068,1.,0.965925826289068,
1.,0.965925826289068,1.,0.965925826289068,1.,0.965925826289068,1.,0.965925826289068,
1.,0.965925826289068,1.,0.965925826289068,1.,0.965925826289068,1.,0.965925826289068,
1.,0.965925826289068,1.,0.965925826289068,1.,0.965925826289068,1.,0.965925826289068,
1.,0.965925826289068,1.,0.965925826289068,1.,0.965925826289068,1.,0.965925826289068,
1.,0.965925826289068,1.,0.965925826289068,1.,0.965925826289068,1.,0.965925826289068,
1.,0.965925826289068,1.,0.965925826289068,1.,0.965925826289068,1.,0.965925826289068,
1.,0.965925826289068,1.,0.965925826289068,1.,0.965925826289068,1.,0.965925826289068,
1.,0.965925826289068,1.,0.965925826289068,1.,0.965925826289068,1.,0.965925826289068,
1.,0.965925826289068,1.,0.965925826289068,1.,0.965925826289068,1.,0.965925826289068,
1.,0.965925826289068,1.,0.965925826289068,1.,0.965925826289068,1.,0.965925826289068,
1.,0.965925826289068,1.,0.965925826289068,1.,0.965925826289068,1.,0.965925826289068,
1.,0.965925826289068,1.,0.965925826289068,1.,0.965925826289068,1.,0.965925826289068,
1.,0.965925826289068,1.,0.965925826289068,1.,0.965925826289068,1.,0.965925826289068,
1.,0.965925826289068,1.,0.965925826289068,1.,0.965925826289068,1.,0.965925826289068,
1.,0.965925826289068,1.,0.965925826289068,1.),(1.,0.965925826289068,1.,
0.965925826289068,1.,0.965925826289068,1.,0.965925826289068,1.,0.965925826289068,
1.,0.965925826289068,1.,0.965925826289068,1.,0.965925826289068,1.,0.965925826289068,
1.,0.965925826289068,1.,0.965925826289068,1.,0.965925826289068,1.,0.965925826289068,
1.,0.965925826289068,1.,0.965925826289068,1.,0.965925826289068,1.,0.965925826289068,
1.,0.965925826289068,1.,0.965925826289068,1.,0.965925826289068,1.,0.965925826289068,
1.,0.965925826289068,1.,0.965925826289068,1.,0.965925826289068,1.,0.965925826289068,
1.,0.965925826289068,1.,0.965925826289068,1.,0.965925826289068,1.,0.965925826289068,
1.,0.965925826289068,1.,0.965925826289068,1.,0.965925826289068,1.,0.965925826289068,
1.,0.965925826289068,1.,0.965925826289068,1.,0.965925826289068,1.,0.965925826289068,
1.,0.965925826289068,1.,0.965925826289068,1.,0.965925826289068,1.,0.965925826289068,
1.,0.965925826289068,1.,0.965925826289068,1.,0.965925826289068,1.,0.965925826289068,
1.,0.965925826289068,1.,0.965925826289068,1.,0.965925826289068,1.,0.965925826289068,
1.,0.965925826289068,1.,0.965925826289068,1.,0.965925826289068,1.,0.965925826289068,
1.,0.965925826289068,1.,0.965925826289068,1.,0.965925826289068,1.,0.965925826289068,
1.,0.965925826289068,1.,0.965925826289068,1.,0.965925826289068,1.,0.965925826289068,
1.,0.965925826289068,1.,0.965925826289068,1.,0.965925826289068,1.,0.965925826289068,
1.,0.965925826289068,1.,0.965925826289068,1.,0.965925826289068,1.,0.965925826289068,
1.,0.965925826289068,1.,0.965925826289068,1.,0.965925826289068,1.)))
REPRESENTATION_ITEM('')
SURFACE()
);
#179=(
BOUNDED_SURFACE()
B_SPLINE_SURFACE(1,2,((#14185,#14186,#14187,#14188,#14189,#14190,#14191,
#14192,#14193,#14194,#14195,#14196,#14197,#14198,#14199,#14200,#14201,#14202,
#14203,#14204,#14205,#14206,#14207,#14208,#14209,#14210,#14211,#14212,#14213,
#14214,#14215,#14216,#14217,#14218,#14219,#14220,#14221,#14222,#14223,#14224,
#14225,#14226,#14227,#14228,#14229,#14230,#14231,#14232,#14233,#14234,#14235,
#14236,#14237,#14238,#14239,#14240,#14241,#14242,#14243,#14244,#14245,#14246,
#14247,#14248,#14249,#14250,#14251,#14252,#14253,#14254,#14255,#14256,#14257,
#14258,#14259,#14260,#14261,#14262,#14263,#14264,#14265,#14266,#14267,#14268,
#14269,#14270,#14271,#14272,#14273,#14274,#14275,#14276,#14277,#14278,#14279,
#14280,#14281,#14282,#14283,#14284,#14285,#14286,#14287,#14288,#14289,#14290,
#14291,#14292,#14293,#14294,#14295,#14296,#14297,#14298,#14299,#14300,#14301,
#14302,#14303,#14304,#14305,#14306,#14307,#14308,#14309,#14310,#14311,#14312,
#14313,#14314,#14315,#14316,#14317,#14318,#14319,#14320,#14321,#14322,#14323,
#14324,#14325,#14326,#14327,#14328,#14329),(#14330,#14331,#14332,#14333,
#14334,#14335,#14336,#14337,#14338,#14339,#14340,#14341,#14342,#14343,#14344,
#14345,#14346,#14347,#14348,#14349,#14350,#14351,#14352,#14353,#14354,#14355,
#14356,#14357,#14358,#14359,#14360,#14361,#14362,#14363,#14364,#14365,#14366,
#14367,#14368,#14369,#14370,#14371,#14372,#14373,#14374,#14375,#14376,#14377,
#14378,#14379,#14380,#14381,#14382,#14383,#14384,#14385,#14386,#14387,#14388,
#14389,#14390,#14391,#14392,#14393,#14394,#14395,#14396,#14397,#14398,#14399,
#14400,#14401,#14402,#14403,#14404,#14405,#14406,#14407,#14408,#14409,#14410,
#14411,#14412,#14413,#14414,#14415,#14416,#14417,#14418,#14419,#14420,#14421,
#14422,#14423,#14424,#14425,#14426,#14427,#14428,#14429,#14430,#14431,#14432,
#14433,#14434,#14435,#14436,#14437,#14438,#14439,#14440,#14441,#14442,#14443,
#14444,#14445,#14446,#14447,#14448,#14449,#14450,#14451,#14452,#14453,#14454,
#14455,#14456,#14457,#14458,#14459,#14460,#14461,#14462,#14463,#14464,#14465,
#14466,#14467,#14468,#14469,#14470,#14471,#14472,#14473,#14474)),
 .UNSPECIFIED.,.F.,.F.,.F.)
B_SPLINE_SURFACE_WITH_KNOTS((2,2),(3,2,2,2,2,2,2,2,2,2,2,2,2,2,2,2,2,2,
2,2,2,2,2,2,2,2,2,2,2,2,2,2,2,2,2,2,2,2,2,2,2,2,2,2,2,2,2,2,2,2,2,2,2,2,
2,2,2,2,2,2,2,2,2,2,2,2,2,2,2,2,2,2,3),(0.,1.),(0.,0.0138888888888889,0.0277777777777778,
0.0416666666666667,0.0555555555555556,0.0694444444444444,0.0833333333333333,
0.0972222222222222,0.111111111111111,0.125,0.138888888888889,0.152777777777778,
0.166666666666667,0.180555555555556,0.194444444444444,0.208333333333333,
0.222222222222222,0.236111111111111,0.25,0.263888888888889,0.277777777777778,
0.291666666666667,0.305555555555556,0.319444444444444,0.333333333333333,
0.347222222222222,0.361111111111111,0.375,0.388888888888889,0.402777777777778,
0.416666666666667,0.430555555555556,0.444444444444444,0.458333333333333,
0.472222222222222,0.486111111111111,0.5,0.513888888888889,0.527777777777778,
0.541666666666667,0.555555555555556,0.569444444444444,0.583333333333333,
0.597222222222222,0.611111111111111,0.625,0.638888888888889,0.652777777777778,
0.666666666666667,0.680555555555556,0.694444444444444,0.708333333333333,
0.722222222222222,0.736111111111111,0.75,0.763888888888889,0.777777777777778,
0.791666666666667,0.805555555555556,0.819444444444444,0.833333333333333,
0.847222222222222,0.861111111111111,0.875,0.888888888888889,0.902777777777778,
0.916666666666667,0.930555555555556,0.944444444444444,0.958333333333333,
0.972222222222222,0.986111111111111,1.),.UNSPECIFIED.)
GEOMETRIC_REPRESENTATION_ITEM()
RATIONAL_B_SPLINE_SURFACE(((1.,0.965925826289068,1.,0.965925826289068,1.,
0.965925826289068,1.,0.965925826289068,1.,0.965925826289068,1.,0.965925826289068,
1.,0.965925826289068,1.,0.965925826289068,1.,0.965925826289068,1.,0.965925826289068,
1.,0.965925826289068,1.,0.965925826289068,1.,0.965925826289068,1.,0.965925826289068,
1.,0.965925826289068,1.,0.965925826289068,1.,0.965925826289068,1.,0.965925826289068,
1.,0.965925826289068,1.,0.965925826289068,1.,0.965925826289068,1.,0.965925826289068,
1.,0.965925826289068,1.,0.965925826289068,1.,0.965925826289068,1.,0.965925826289068,
1.,0.965925826289068,1.,0.965925826289068,1.,0.965925826289068,1.,0.965925826289068,
1.,0.965925826289068,1.,0.965925826289068,1.,0.965925826289068,1.,0.965925826289068,
1.,0.965925826289068,1.,0.965925826289068,1.,0.965925826289068,1.,0.965925826289068,
1.,0.965925826289068,1.,0.965925826289068,1.,0.965925826289068,1.,0.965925826289068,
1.,0.965925826289068,1.,0.965925826289068,1.,0.965925826289068,1.,0.965925826289068,
1.,0.965925826289068,1.,0.965925826289068,1.,0.965925826289068,1.,0.965925826289068,
1.,0.965925826289068,1.,0.965925826289068,1.,0.965925826289068,1.,0.965925826289068,
1.,0.965925826289068,1.,0.965925826289068,1.,0.965925826289068,1.,0.965925826289068,
1.,0.965925826289068,1.,0.965925826289068,1.,0.965925826289068,1.,0.965925826289068,
1.,0.965925826289068,1.,0.965925826289068,1.,0.965925826289068,1.,0.965925826289068,
1.,0.965925826289068,1.,0.965925826289068,1.,0.965925826289068,1.,0.965925826289068,
1.,0.965925826289068,1.,0.965925826289068,1.),(1.,0.965925826289068,1.,
0.965925826289068,1.,0.965925826289068,1.,0.965925826289068,1.,0.965925826289068,
1.,0.965925826289068,1.,0.965925826289068,1.,0.965925826289068,1.,0.965925826289068,
1.,0.965925826289068,1.,0.965925826289068,1.,0.965925826289068,1.,0.965925826289068,
1.,0.965925826289068,1.,0.965925826289068,1.,0.965925826289068,1.,0.965925826289068,
1.,0.965925826289068,1.,0.965925826289068,1.,0.965925826289068,1.,0.965925826289068,
1.,0.965925826289068,1.,0.965925826289068,1.,0.965925826289068,1.,0.965925826289068,
1.,0.965925826289068,1.,0.965925826289068,1.,0.965925826289068,1.,0.965925826289068,
1.,0.965925826289068,1.,0.965925826289068,1.,0.965925826289068,1.,0.965925826289068,
1.,0.965925826289068,1.,0.965925826289068,1.,0.965925826289068,1.,0.965925826289068,
1.,0.965925826289068,1.,0.965925826289068,1.,0.965925826289068,1.,0.965925826289068,
1.,0.965925826289068,1.,0.965925826289068,1.,0.965925826289068,1.,0.965925826289068,
1.,0.965925826289068,1.,0.965925826289068,1.,0.965925826289068,1.,0.965925826289068,
1.,0.965925826289068,1.,0.965925826289068,1.,0.965925826289068,1.,0.965925826289068,
1.,0.965925826289068,1.,0.965925826289068,1.,0.965925826289068,1.,0.965925826289068,
1.,0.965925826289068,1.,0.965925826289068,1.,0.965925826289068,1.,0.965925826289068,
1.,0.965925826289068,1.,0.965925826289068,1.,0.965925826289068,1.,0.965925826289068,
1.,0.965925826289068,1.,0.965925826289068,1.,0.965925826289068,1.,0.965925826289068,
1.,0.965925826289068,1.,0.965925826289068,1.,0.965925826289068,1.)))
REPRESENTATION_ITEM('')
SURFACE()
);
#180=(
BOUNDED_SURFACE()
B_SPLINE_SURFACE(1,2,((#14483,#14484,#14485,#14486,#14487,#14488,#14489,
#14490,#14491,#14492,#14493,#14494,#14495,#14496,#14497,#14498,#14499,#14500,
#14501,#14502,#14503,#14504,#14505,#14506,#14507,#14508,#14509,#14510,#14511,
#14512,#14513,#14514,#14515,#14516,#14517,#14518,#14519,#14520,#14521,#14522,
#14523,#14524,#14525,#14526,#14527,#14528,#14529,#14530,#14531,#14532,#14533,
#14534,#14535,#14536,#14537,#14538,#14539,#14540,#14541,#14542,#14543,#14544,
#14545,#14546,#14547,#14548,#14549,#14550,#14551,#14552,#14553,#14554,#14555,
#14556,#14557,#14558,#14559,#14560,#14561,#14562,#14563,#14564,#14565,#14566,
#14567,#14568,#14569,#14570,#14571,#14572,#14573,#14574,#14575,#14576,#14577,
#14578,#14579,#14580,#14581,#14582,#14583,#14584,#14585,#14586,#14587,#14588,
#14589,#14590,#14591,#14592,#14593,#14594,#14595,#14596,#14597,#14598,#14599,
#14600,#14601,#14602,#14603,#14604,#14605,#14606,#14607,#14608,#14609,#14610,
#14611,#14612,#14613,#14614,#14615,#14616,#14617,#14618,#14619,#14620,#14621,
#14622,#14623,#14624,#14625,#14626,#14627),(#14628,#14629,#14630,#14631,
#14632,#14633,#14634,#14635,#14636,#14637,#14638,#14639,#14640,#14641,#14642,
#14643,#14644,#14645,#14646,#14647,#14648,#14649,#14650,#14651,#14652,#14653,
#14654,#14655,#14656,#14657,#14658,#14659,#14660,#14661,#14662,#14663,#14664,
#14665,#14666,#14667,#14668,#14669,#14670,#14671,#14672,#14673,#14674,#14675,
#14676,#14677,#14678,#14679,#14680,#14681,#14682,#14683,#14684,#14685,#14686,
#14687,#14688,#14689,#14690,#14691,#14692,#14693,#14694,#14695,#14696,#14697,
#14698,#14699,#14700,#14701,#14702,#14703,#14704,#14705,#14706,#14707,#14708,
#14709,#14710,#14711,#14712,#14713,#14714,#14715,#14716,#14717,#14718,#14719,
#14720,#14721,#14722,#14723,#14724,#14725,#14726,#14727,#14728,#14729,#14730,
#14731,#14732,#14733,#14734,#14735,#14736,#14737,#14738,#14739,#14740,#14741,
#14742,#14743,#14744,#14745,#14746,#14747,#14748,#14749,#14750,#14751,#14752,
#14753,#14754,#14755,#14756,#14757,#14758,#14759,#14760,#14761,#14762,#14763,
#14764,#14765,#14766,#14767,#14768,#14769,#14770,#14771,#14772)),
 .UNSPECIFIED.,.F.,.F.,.F.)
B_SPLINE_SURFACE_WITH_KNOTS((2,2),(3,2,2,2,2,2,2,2,2,2,2,2,2,2,2,2,2,2,
2,2,2,2,2,2,2,2,2,2,2,2,2,2,2,2,2,2,2,2,2,2,2,2,2,2,2,2,2,2,2,2,2,2,2,2,
2,2,2,2,2,2,2,2,2,2,2,2,2,2,2,2,2,2,3),(0.,1.),(0.,0.0138888888888889,0.0277777777777778,
0.0416666666666667,0.0555555555555556,0.0694444444444444,0.0833333333333333,
0.0972222222222222,0.111111111111111,0.125,0.138888888888889,0.152777777777778,
0.166666666666667,0.180555555555556,0.194444444444444,0.208333333333333,
0.222222222222222,0.236111111111111,0.25,0.263888888888889,0.277777777777778,
0.291666666666667,0.305555555555556,0.319444444444444,0.333333333333333,
0.347222222222222,0.361111111111111,0.375,0.388888888888889,0.402777777777778,
0.416666666666667,0.430555555555556,0.444444444444444,0.458333333333333,
0.472222222222222,0.486111111111111,0.5,0.513888888888889,0.527777777777778,
0.541666666666667,0.555555555555556,0.569444444444444,0.583333333333333,
0.597222222222222,0.611111111111111,0.625,0.638888888888889,0.652777777777778,
0.666666666666667,0.680555555555556,0.694444444444444,0.708333333333333,
0.722222222222222,0.736111111111111,0.75,0.763888888888889,0.777777777777778,
0.791666666666667,0.805555555555556,0.819444444444444,0.833333333333333,
0.847222222222222,0.861111111111111,0.875,0.888888888888889,0.902777777777778,
0.916666666666667,0.930555555555556,0.944444444444444,0.958333333333333,
0.972222222222222,0.986111111111111,1.),.UNSPECIFIED.)
GEOMETRIC_REPRESENTATION_ITEM()
RATIONAL_B_SPLINE_SURFACE(((1.,0.965925826289068,1.,0.965925826289068,1.,
0.965925826289068,1.,0.965925826289068,1.,0.965925826289068,1.,0.965925826289068,
1.,0.965925826289068,1.,0.965925826289068,1.,0.965925826289068,1.,0.965925826289068,
1.,0.965925826289068,1.,0.965925826289068,1.,0.965925826289068,1.,0.965925826289068,
1.,0.965925826289068,1.,0.965925826289068,1.,0.965925826289068,1.,0.965925826289068,
1.,0.965925826289068,1.,0.965925826289068,1.,0.965925826289068,1.,0.965925826289068,
1.,0.965925826289068,1.,0.965925826289068,1.,0.965925826289068,1.,0.965925826289068,
1.,0.965925826289068,1.,0.965925826289068,1.,0.965925826289068,1.,0.965925826289068,
1.,0.965925826289068,1.,0.965925826289068,1.,0.965925826289068,1.,0.965925826289068,
1.,0.965925826289068,1.,0.965925826289068,1.,0.965925826289068,1.,0.965925826289068,
1.,0.965925826289068,1.,0.965925826289068,1.,0.965925826289068,1.,0.965925826289068,
1.,0.965925826289068,1.,0.965925826289068,1.,0.965925826289068,1.,0.965925826289068,
1.,0.965925826289068,1.,0.965925826289068,1.,0.965925826289068,1.,0.965925826289068,
1.,0.965925826289068,1.,0.965925826289068,1.,0.965925826289068,1.,0.965925826289068,
1.,0.965925826289068,1.,0.965925826289068,1.,0.965925826289068,1.,0.965925826289068,
1.,0.965925826289068,1.,0.965925826289068,1.,0.965925826289068,1.,0.965925826289068,
1.,0.965925826289068,1.,0.965925826289068,1.,0.965925826289068,1.,0.965925826289068,
1.,0.965925826289068,1.,0.965925826289068,1.,0.965925826289068,1.,0.965925826289068,
1.,0.965925826289068,1.,0.965925826289068,1.),(1.,0.965925826289068,1.,
0.965925826289068,1.,0.965925826289068,1.,0.965925826289068,1.,0.965925826289068,
1.,0.965925826289068,1.,0.965925826289068,1.,0.965925826289068,1.,0.965925826289068,
1.,0.965925826289068,1.,0.965925826289068,1.,0.965925826289068,1.,0.965925826289068,
1.,0.965925826289068,1.,0.965925826289068,1.,0.965925826289068,1.,0.965925826289068,
1.,0.965925826289068,1.,0.965925826289068,1.,0.965925826289068,1.,0.965925826289068,
1.,0.965925826289068,1.,0.965925826289068,1.,0.965925826289068,1.,0.965925826289068,
1.,0.965925826289068,1.,0.965925826289068,1.,0.965925826289068,1.,0.965925826289068,
1.,0.965925826289068,1.,0.965925826289068,1.,0.965925826289068,1.,0.965925826289068,
1.,0.965925826289068,1.,0.965925826289068,1.,0.965925826289068,1.,0.965925826289068,
1.,0.965925826289068,1.,0.965925826289068,1.,0.965925826289068,1.,0.965925826289068,
1.,0.965925826289068,1.,0.965925826289068,1.,0.965925826289068,1.,0.965925826289068,
1.,0.965925826289068,1.,0.965925826289068,1.,0.965925826289068,1.,0.965925826289068,
1.,0.965925826289068,1.,0.965925826289068,1.,0.965925826289068,1.,0.965925826289068,
1.,0.965925826289068,1.,0.965925826289068,1.,0.965925826289068,1.,0.965925826289068,
1.,0.965925826289068,1.,0.965925826289068,1.,0.965925826289068,1.,0.965925826289068,
1.,0.965925826289068,1.,0.965925826289068,1.,0.965925826289068,1.,0.965925826289068,
1.,0.965925826289068,1.,0.965925826289068,1.,0.965925826289068,1.,0.965925826289068,
1.,0.965925826289068,1.,0.965925826289068,1.,0.965925826289068,1.)))
REPRESENTATION_ITEM('')
SURFACE()
);
#181=(
BOUNDED_SURFACE()
B_SPLINE_SURFACE(1,2,((#14781,#14782,#14783,#14784,#14785,#14786,#14787,
#14788,#14789,#14790,#14791,#14792,#14793,#14794,#14795,#14796,#14797,#14798,
#14799,#14800,#14801,#14802,#14803,#14804,#14805,#14806,#14807,#14808,#14809,
#14810,#14811,#14812,#14813,#14814,#14815,#14816,#14817,#14818,#14819,#14820,
#14821,#14822,#14823,#14824,#14825,#14826,#14827,#14828,#14829,#14830,#14831,
#14832,#14833,#14834,#14835,#14836,#14837,#14838,#14839,#14840,#14841,#14842,
#14843,#14844,#14845,#14846,#14847,#14848,#14849,#14850,#14851,#14852,#14853,
#14854,#14855,#14856,#14857,#14858,#14859,#14860,#14861,#14862,#14863,#14864,
#14865,#14866,#14867,#14868,#14869,#14870,#14871,#14872,#14873,#14874,#14875,
#14876,#14877,#14878,#14879,#14880,#14881,#14882,#14883,#14884,#14885,#14886,
#14887,#14888,#14889,#14890,#14891,#14892,#14893,#14894,#14895,#14896,#14897,
#14898,#14899,#14900,#14901,#14902,#14903,#14904,#14905,#14906,#14907,#14908,
#14909,#14910,#14911,#14912,#14913,#14914,#14915,#14916,#14917,#14918,#14919,
#14920,#14921,#14922,#14923,#14924,#14925),(#14926,#14927,#14928,#14929,
#14930,#14931,#14932,#14933,#14934,#14935,#14936,#14937,#14938,#14939,#14940,
#14941,#14942,#14943,#14944,#14945,#14946,#14947,#14948,#14949,#14950,#14951,
#14952,#14953,#14954,#14955,#14956,#14957,#14958,#14959,#14960,#14961,#14962,
#14963,#14964,#14965,#14966,#14967,#14968,#14969,#14970,#14971,#14972,#14973,
#14974,#14975,#14976,#14977,#14978,#14979,#14980,#14981,#14982,#14983,#14984,
#14985,#14986,#14987,#14988,#14989,#14990,#14991,#14992,#14993,#14994,#14995,
#14996,#14997,#14998,#14999,#15000,#15001,#15002,#15003,#15004,#15005,#15006,
#15007,#15008,#15009,#15010,#15011,#15012,#15013,#15014,#15015,#15016,#15017,
#15018,#15019,#15020,#15021,#15022,#15023,#15024,#15025,#15026,#15027,#15028,
#15029,#15030,#15031,#15032,#15033,#15034,#15035,#15036,#15037,#15038,#15039,
#15040,#15041,#15042,#15043,#15044,#15045,#15046,#15047,#15048,#15049,#15050,
#15051,#15052,#15053,#15054,#15055,#15056,#15057,#15058,#15059,#15060,#15061,
#15062,#15063,#15064,#15065,#15066,#15067,#15068,#15069,#15070)),
 .UNSPECIFIED.,.F.,.F.,.F.)
B_SPLINE_SURFACE_WITH_KNOTS((2,2),(3,2,2,2,2,2,2,2,2,2,2,2,2,2,2,2,2,2,
2,2,2,2,2,2,2,2,2,2,2,2,2,2,2,2,2,2,2,2,2,2,2,2,2,2,2,2,2,2,2,2,2,2,2,2,
2,2,2,2,2,2,2,2,2,2,2,2,2,2,2,2,2,2,3),(0.,1.),(0.,0.0138888888888889,0.0277777777777778,
0.0416666666666667,0.0555555555555556,0.0694444444444444,0.0833333333333333,
0.0972222222222222,0.111111111111111,0.125,0.138888888888889,0.152777777777778,
0.166666666666667,0.180555555555556,0.194444444444444,0.208333333333333,
0.222222222222222,0.236111111111111,0.25,0.263888888888889,0.277777777777778,
0.291666666666667,0.305555555555556,0.319444444444444,0.333333333333333,
0.347222222222222,0.361111111111111,0.375,0.388888888888889,0.402777777777778,
0.416666666666667,0.430555555555556,0.444444444444444,0.458333333333333,
0.472222222222222,0.486111111111111,0.5,0.513888888888889,0.527777777777778,
0.541666666666667,0.555555555555556,0.569444444444444,0.583333333333333,
0.597222222222222,0.611111111111111,0.625,0.638888888888889,0.652777777777778,
0.666666666666667,0.680555555555556,0.694444444444444,0.708333333333333,
0.722222222222222,0.736111111111111,0.75,0.763888888888889,0.777777777777778,
0.791666666666667,0.805555555555556,0.819444444444444,0.833333333333333,
0.847222222222222,0.861111111111111,0.875,0.888888888888889,0.902777777777778,
0.916666666666667,0.930555555555556,0.944444444444444,0.958333333333333,
0.972222222222222,0.986111111111111,1.),.UNSPECIFIED.)
GEOMETRIC_REPRESENTATION_ITEM()
RATIONAL_B_SPLINE_SURFACE(((1.,0.965925826289068,1.,0.965925826289068,1.,
0.965925826289068,1.,0.965925826289068,1.,0.965925826289068,1.,0.965925826289068,
1.,0.965925826289068,1.,0.965925826289068,1.,0.965925826289068,1.,0.965925826289068,
1.,0.965925826289068,1.,0.965925826289068,1.,0.965925826289068,1.,0.965925826289068,
1.,0.965925826289068,1.,0.965925826289068,1.,0.965925826289068,1.,0.965925826289068,
1.,0.965925826289068,1.,0.965925826289068,1.,0.965925826289068,1.,0.965925826289068,
1.,0.965925826289068,1.,0.965925826289068,1.,0.965925826289068,1.,0.965925826289068,
1.,0.965925826289068,1.,0.965925826289068,1.,0.965925826289068,1.,0.965925826289068,
1.,0.965925826289068,1.,0.965925826289068,1.,0.965925826289068,1.,0.965925826289068,
1.,0.965925826289068,1.,0.965925826289068,1.,0.965925826289068,1.,0.965925826289068,
1.,0.965925826289068,1.,0.965925826289068,1.,0.965925826289068,1.,0.965925826289068,
1.,0.965925826289068,1.,0.965925826289068,1.,0.965925826289068,1.,0.965925826289068,
1.,0.965925826289068,1.,0.965925826289068,1.,0.965925826289068,1.,0.965925826289068,
1.,0.965925826289068,1.,0.965925826289068,1.,0.965925826289068,1.,0.965925826289068,
1.,0.965925826289068,1.,0.965925826289068,1.,0.965925826289068,1.,0.965925826289068,
1.,0.965925826289068,1.,0.965925826289068,1.,0.965925826289068,1.,0.965925826289068,
1.,0.965925826289068,1.,0.965925826289068,1.,0.965925826289068,1.,0.965925826289068,
1.,0.965925826289068,1.,0.965925826289068,1.,0.965925826289068,1.,0.965925826289068,
1.,0.965925826289068,1.,0.965925826289068,1.),(1.,0.965925826289068,1.,
0.965925826289068,1.,0.965925826289068,1.,0.965925826289068,1.,0.965925826289068,
1.,0.965925826289068,1.,0.965925826289068,1.,0.965925826289068,1.,0.965925826289068,
1.,0.965925826289068,1.,0.965925826289068,1.,0.965925826289068,1.,0.965925826289068,
1.,0.965925826289068,1.,0.965925826289068,1.,0.965925826289068,1.,0.965925826289068,
1.,0.965925826289068,1.,0.965925826289068,1.,0.965925826289068,1.,0.965925826289068,
1.,0.965925826289068,1.,0.965925826289068,1.,0.965925826289068,1.,0.965925826289068,
1.,0.965925826289068,1.,0.965925826289068,1.,0.965925826289068,1.,0.965925826289068,
1.,0.965925826289068,1.,0.965925826289068,1.,0.965925826289068,1.,0.965925826289068,
1.,0.965925826289068,1.,0.965925826289068,1.,0.965925826289068,1.,0.965925826289068,
1.,0.965925826289068,1.,0.965925826289068,1.,0.965925826289068,1.,0.965925826289068,
1.,0.965925826289068,1.,0.965925826289068,1.,0.965925826289068,1.,0.965925826289068,
1.,0.965925826289068,1.,0.965925826289068,1.,0.965925826289068,1.,0.965925826289068,
1.,0.965925826289068,1.,0.965925826289068,1.,0.965925826289068,1.,0.965925826289068,
1.,0.965925826289068,1.,0.965925826289068,1.,0.965925826289068,1.,0.965925826289068,
1.,0.965925826289068,1.,0.965925826289068,1.,0.965925826289068,1.,0.965925826289068,
1.,0.965925826289068,1.,0.965925826289068,1.,0.965925826289068,1.,0.965925826289068,
1.,0.965925826289068,1.,0.965925826289068,1.,0.965925826289068,1.,0.965925826289068,
1.,0.965925826289068,1.,0.965925826289068,1.,0.965925826289068,1.)))
REPRESENTATION_ITEM('')
SURFACE()
);
#182=(
BOUNDED_SURFACE()
B_SPLINE_SURFACE(1,2,((#15079,#15080,#15081,#15082,#15083,#15084,#15085,
#15086,#15087,#15088,#15089,#15090,#15091,#15092,#15093,#15094,#15095,#15096,
#15097,#15098,#15099,#15100,#15101,#15102,#15103,#15104,#15105,#15106,#15107,
#15108,#15109,#15110,#15111,#15112,#15113,#15114,#15115,#15116,#15117,#15118,
#15119,#15120,#15121,#15122,#15123,#15124,#15125,#15126,#15127,#15128,#15129,
#15130,#15131,#15132,#15133,#15134,#15135,#15136,#15137,#15138,#15139,#15140,
#15141,#15142,#15143,#15144,#15145,#15146,#15147,#15148,#15149,#15150,#15151,
#15152,#15153,#15154,#15155,#15156,#15157,#15158,#15159,#15160,#15161,#15162,
#15163,#15164,#15165,#15166,#15167,#15168,#15169,#15170,#15171,#15172,#15173,
#15174,#15175,#15176,#15177,#15178,#15179,#15180,#15181,#15182,#15183,#15184,
#15185,#15186,#15187,#15188,#15189,#15190,#15191,#15192,#15193,#15194,#15195,
#15196,#15197,#15198,#15199,#15200,#15201,#15202,#15203,#15204,#15205,#15206,
#15207,#15208,#15209,#15210,#15211,#15212,#15213,#15214,#15215,#15216,#15217,
#15218,#15219,#15220,#15221,#15222,#15223),(#15224,#15225,#15226,#15227,
#15228,#15229,#15230,#15231,#15232,#15233,#15234,#15235,#15236,#15237,#15238,
#15239,#15240,#15241,#15242,#15243,#15244,#15245,#15246,#15247,#15248,#15249,
#15250,#15251,#15252,#15253,#15254,#15255,#15256,#15257,#15258,#15259,#15260,
#15261,#15262,#15263,#15264,#15265,#15266,#15267,#15268,#15269,#15270,#15271,
#15272,#15273,#15274,#15275,#15276,#15277,#15278,#15279,#15280,#15281,#15282,
#15283,#15284,#15285,#15286,#15287,#15288,#15289,#15290,#15291,#15292,#15293,
#15294,#15295,#15296,#15297,#15298,#15299,#15300,#15301,#15302,#15303,#15304,
#15305,#15306,#15307,#15308,#15309,#15310,#15311,#15312,#15313,#15314,#15315,
#15316,#15317,#15318,#15319,#15320,#15321,#15322,#15323,#15324,#15325,#15326,
#15327,#15328,#15329,#15330,#15331,#15332,#15333,#15334,#15335,#15336,#15337,
#15338,#15339,#15340,#15341,#15342,#15343,#15344,#15345,#15346,#15347,#15348,
#15349,#15350,#15351,#15352,#15353,#15354,#15355,#15356,#15357,#15358,#15359,
#15360,#15361,#15362,#15363,#15364,#15365,#15366,#15367,#15368)),
 .UNSPECIFIED.,.F.,.F.,.F.)
B_SPLINE_SURFACE_WITH_KNOTS((2,2),(3,2,2,2,2,2,2,2,2,2,2,2,2,2,2,2,2,2,
2,2,2,2,2,2,2,2,2,2,2,2,2,2,2,2,2,2,2,2,2,2,2,2,2,2,2,2,2,2,2,2,2,2,2,2,
2,2,2,2,2,2,2,2,2,2,2,2,2,2,2,2,2,2,3),(0.,1.),(0.,0.0138888888888889,0.0277777777777778,
0.0416666666666667,0.0555555555555556,0.0694444444444444,0.0833333333333333,
0.0972222222222222,0.111111111111111,0.125,0.138888888888889,0.152777777777778,
0.166666666666667,0.180555555555556,0.194444444444444,0.208333333333333,
0.222222222222222,0.236111111111111,0.25,0.263888888888889,0.277777777777778,
0.291666666666667,0.305555555555556,0.319444444444444,0.333333333333333,
0.347222222222222,0.361111111111111,0.375,0.388888888888889,0.402777777777778,
0.416666666666667,0.430555555555556,0.444444444444444,0.458333333333333,
0.472222222222222,0.486111111111111,0.5,0.513888888888889,0.527777777777778,
0.541666666666667,0.555555555555556,0.569444444444444,0.583333333333333,
0.597222222222222,0.611111111111111,0.625,0.638888888888889,0.652777777777778,
0.666666666666667,0.680555555555556,0.694444444444444,0.708333333333333,
0.722222222222222,0.736111111111111,0.75,0.763888888888889,0.777777777777778,
0.791666666666667,0.805555555555556,0.819444444444444,0.833333333333333,
0.847222222222222,0.861111111111111,0.875,0.888888888888889,0.902777777777778,
0.916666666666667,0.930555555555556,0.944444444444444,0.958333333333333,
0.972222222222222,0.986111111111111,1.),.UNSPECIFIED.)
GEOMETRIC_REPRESENTATION_ITEM()
RATIONAL_B_SPLINE_SURFACE(((1.,0.965925826289068,1.,0.965925826289068,1.,
0.965925826289068,1.,0.965925826289068,1.,0.965925826289068,1.,0.965925826289068,
1.,0.965925826289068,1.,0.965925826289068,1.,0.965925826289068,1.,0.965925826289068,
1.,0.965925826289068,1.,0.965925826289068,1.,0.965925826289068,1.,0.965925826289068,
1.,0.965925826289068,1.,0.965925826289068,1.,0.965925826289068,1.,0.965925826289068,
1.,0.965925826289068,1.,0.965925826289068,1.,0.965925826289068,1.,0.965925826289068,
1.,0.965925826289068,1.,0.965925826289068,1.,0.965925826289068,1.,0.965925826289068,
1.,0.965925826289068,1.,0.965925826289068,1.,0.965925826289068,1.,0.965925826289068,
1.,0.965925826289068,1.,0.965925826289068,1.,0.965925826289068,1.,0.965925826289068,
1.,0.965925826289068,1.,0.965925826289068,1.,0.965925826289068,1.,0.965925826289068,
1.,0.965925826289068,1.,0.965925826289068,1.,0.965925826289068,1.,0.965925826289068,
1.,0.965925826289068,1.,0.965925826289068,1.,0.965925826289068,1.,0.965925826289068,
1.,0.965925826289068,1.,0.965925826289068,1.,0.965925826289068,1.,0.965925826289068,
1.,0.965925826289068,1.,0.965925826289068,1.,0.965925826289068,1.,0.965925826289068,
1.,0.965925826289068,1.,0.965925826289068,1.,0.965925826289068,1.,0.965925826289068,
1.,0.965925826289068,1.,0.965925826289068,1.,0.965925826289068,1.,0.965925826289068,
1.,0.965925826289068,1.,0.965925826289068,1.,0.965925826289068,1.,0.965925826289068,
1.,0.965925826289068,1.,0.965925826289068,1.,0.965925826289068,1.,0.965925826289068,
1.,0.965925826289068,1.,0.965925826289068,1.),(1.,0.965925826289068,1.,
0.965925826289068,1.,0.965925826289068,1.,0.965925826289068,1.,0.965925826289068,
1.,0.965925826289068,1.,0.965925826289068,1.,0.965925826289068,1.,0.965925826289068,
1.,0.965925826289068,1.,0.965925826289068,1.,0.965925826289068,1.,0.965925826289068,
1.,0.965925826289068,1.,0.965925826289068,1.,0.965925826289068,1.,0.965925826289068,
1.,0.965925826289068,1.,0.965925826289068,1.,0.965925826289068,1.,0.965925826289068,
1.,0.965925826289068,1.,0.965925826289068,1.,0.965925826289068,1.,0.965925826289068,
1.,0.965925826289068,1.,0.965925826289068,1.,0.965925826289068,1.,0.965925826289068,
1.,0.965925826289068,1.,0.965925826289068,1.,0.965925826289068,1.,0.965925826289068,
1.,0.965925826289068,1.,0.965925826289068,1.,0.965925826289068,1.,0.965925826289068,
1.,0.965925826289068,1.,0.965925826289068,1.,0.965925826289068,1.,0.965925826289068,
1.,0.965925826289068,1.,0.965925826289068,1.,0.965925826289068,1.,0.965925826289068,
1.,0.965925826289068,1.,0.965925826289068,1.,0.965925826289068,1.,0.965925826289068,
1.,0.965925826289068,1.,0.965925826289068,1.,0.965925826289068,1.,0.965925826289068,
1.,0.965925826289068,1.,0.965925826289068,1.,0.965925826289068,1.,0.965925826289068,
1.,0.965925826289068,1.,0.965925826289068,1.,0.965925826289068,1.,0.965925826289068,
1.,0.965925826289068,1.,0.965925826289068,1.,0.965925826289068,1.,0.965925826289068,
1.,0.965925826289068,1.,0.965925826289068,1.,0.965925826289068,1.,0.965925826289068,
1.,0.965925826289068,1.,0.965925826289068,1.,0.965925826289068,1.)))
REPRESENTATION_ITEM('')
SURFACE()
);
#183=(
BOUNDED_SURFACE()
B_SPLINE_SURFACE(1,2,((#15377,#15378,#15379,#15380,#15381,#15382,#15383,
#15384,#15385,#15386,#15387,#15388,#15389,#15390,#15391,#15392,#15393,#15394,
#15395,#15396,#15397,#15398,#15399,#15400,#15401,#15402,#15403,#15404,#15405,
#15406,#15407,#15408,#15409,#15410,#15411,#15412,#15413,#15414,#15415,#15416,
#15417,#15418,#15419,#15420,#15421,#15422,#15423,#15424,#15425,#15426,#15427,
#15428,#15429,#15430,#15431,#15432,#15433,#15434,#15435,#15436,#15437,#15438,
#15439,#15440,#15441,#15442,#15443,#15444,#15445,#15446,#15447,#15448,#15449,
#15450,#15451,#15452,#15453,#15454,#15455,#15456,#15457,#15458,#15459,#15460,
#15461,#15462,#15463,#15464,#15465,#15466,#15467,#15468,#15469,#15470,#15471,
#15472,#15473,#15474,#15475,#15476,#15477,#15478,#15479,#15480,#15481,#15482,
#15483,#15484,#15485,#15486,#15487,#15488,#15489,#15490,#15491,#15492,#15493,
#15494,#15495,#15496,#15497,#15498,#15499,#15500,#15501,#15502,#15503,#15504,
#15505,#15506,#15507,#15508,#15509,#15510,#15511,#15512,#15513,#15514,#15515,
#15516,#15517,#15518,#15519,#15520,#15521),(#15522,#15523,#15524,#15525,
#15526,#15527,#15528,#15529,#15530,#15531,#15532,#15533,#15534,#15535,#15536,
#15537,#15538,#15539,#15540,#15541,#15542,#15543,#15544,#15545,#15546,#15547,
#15548,#15549,#15550,#15551,#15552,#15553,#15554,#15555,#15556,#15557,#15558,
#15559,#15560,#15561,#15562,#15563,#15564,#15565,#15566,#15567,#15568,#15569,
#15570,#15571,#15572,#15573,#15574,#15575,#15576,#15577,#15578,#15579,#15580,
#15581,#15582,#15583,#15584,#15585,#15586,#15587,#15588,#15589,#15590,#15591,
#15592,#15593,#15594,#15595,#15596,#15597,#15598,#15599,#15600,#15601,#15602,
#15603,#15604,#15605,#15606,#15607,#15608,#15609,#15610,#15611,#15612,#15613,
#15614,#15615,#15616,#15617,#15618,#15619,#15620,#15621,#15622,#15623,#15624,
#15625,#15626,#15627,#15628,#15629,#15630,#15631,#15632,#15633,#15634,#15635,
#15636,#15637,#15638,#15639,#15640,#15641,#15642,#15643,#15644,#15645,#15646,
#15647,#15648,#15649,#15650,#15651,#15652,#15653,#15654,#15655,#15656,#15657,
#15658,#15659,#15660,#15661,#15662,#15663,#15664,#15665,#15666)),
 .UNSPECIFIED.,.F.,.F.,.F.)
B_SPLINE_SURFACE_WITH_KNOTS((2,2),(3,2,2,2,2,2,2,2,2,2,2,2,2,2,2,2,2,2,
2,2,2,2,2,2,2,2,2,2,2,2,2,2,2,2,2,2,2,2,2,2,2,2,2,2,2,2,2,2,2,2,2,2,2,2,
2,2,2,2,2,2,2,2,2,2,2,2,2,2,2,2,2,2,3),(0.,1.),(0.,0.0138888888888889,0.0277777777777778,
0.0416666666666667,0.0555555555555556,0.0694444444444444,0.0833333333333333,
0.0972222222222222,0.111111111111111,0.125,0.138888888888889,0.152777777777778,
0.166666666666667,0.180555555555556,0.194444444444444,0.208333333333333,
0.222222222222222,0.236111111111111,0.25,0.263888888888889,0.277777777777778,
0.291666666666667,0.305555555555556,0.319444444444444,0.333333333333333,
0.347222222222222,0.361111111111111,0.375,0.388888888888889,0.402777777777778,
0.416666666666667,0.430555555555556,0.444444444444444,0.458333333333333,
0.472222222222222,0.486111111111111,0.5,0.513888888888889,0.527777777777778,
0.541666666666667,0.555555555555556,0.569444444444444,0.583333333333333,
0.597222222222222,0.611111111111111,0.625,0.638888888888889,0.652777777777778,
0.666666666666667,0.680555555555556,0.694444444444444,0.708333333333333,
0.722222222222222,0.736111111111111,0.75,0.763888888888889,0.777777777777778,
0.791666666666667,0.805555555555556,0.819444444444444,0.833333333333333,
0.847222222222222,0.861111111111111,0.875,0.888888888888889,0.902777777777778,
0.916666666666667,0.930555555555556,0.944444444444444,0.958333333333333,
0.972222222222222,0.986111111111111,1.),.UNSPECIFIED.)
GEOMETRIC_REPRESENTATION_ITEM()
RATIONAL_B_SPLINE_SURFACE(((1.,0.965925826289068,1.,0.965925826289068,1.,
0.965925826289068,1.,0.965925826289068,1.,0.965925826289068,1.,0.965925826289068,
1.,0.965925826289068,1.,0.965925826289068,1.,0.965925826289068,1.,0.965925826289068,
1.,0.965925826289068,1.,0.965925826289068,1.,0.965925826289068,1.,0.965925826289068,
1.,0.965925826289068,1.,0.965925826289068,1.,0.965925826289068,1.,0.965925826289068,
1.,0.965925826289068,1.,0.965925826289068,1.,0.965925826289068,1.,0.965925826289068,
1.,0.965925826289068,1.,0.965925826289068,1.,0.965925826289068,1.,0.965925826289068,
1.,0.965925826289068,1.,0.965925826289068,1.,0.965925826289068,1.,0.965925826289068,
1.,0.965925826289068,1.,0.965925826289068,1.,0.965925826289068,1.,0.965925826289068,
1.,0.965925826289068,1.,0.965925826289068,1.,0.965925826289068,1.,0.965925826289068,
1.,0.965925826289068,1.,0.965925826289068,1.,0.965925826289068,1.,0.965925826289068,
1.,0.965925826289068,1.,0.965925826289068,1.,0.965925826289068,1.,0.965925826289068,
1.,0.965925826289068,1.,0.965925826289068,1.,0.965925826289068,1.,0.965925826289068,
1.,0.965925826289068,1.,0.965925826289068,1.,0.965925826289068,1.,0.965925826289068,
1.,0.965925826289068,1.,0.965925826289068,1.,0.965925826289068,1.,0.965925826289068,
1.,0.965925826289068,1.,0.965925826289068,1.,0.965925826289068,1.,0.965925826289068,
1.,0.965925826289068,1.,0.965925826289068,1.,0.965925826289068,1.,0.965925826289068,
1.,0.965925826289068,1.,0.965925826289068,1.,0.965925826289068,1.,0.965925826289068,
1.,0.965925826289068,1.,0.965925826289068,1.),(1.,0.965925826289068,1.,
0.965925826289068,1.,0.965925826289068,1.,0.965925826289068,1.,0.965925826289068,
1.,0.965925826289068,1.,0.965925826289068,1.,0.965925826289068,1.,0.965925826289068,
1.,0.965925826289068,1.,0.965925826289068,1.,0.965925826289068,1.,0.965925826289068,
1.,0.965925826289068,1.,0.965925826289068,1.,0.965925826289068,1.,0.965925826289068,
1.,0.965925826289068,1.,0.965925826289068,1.,0.965925826289068,1.,0.965925826289068,
1.,0.965925826289068,1.,0.965925826289068,1.,0.965925826289068,1.,0.965925826289068,
1.,0.965925826289068,1.,0.965925826289068,1.,0.965925826289068,1.,0.965925826289068,
1.,0.965925826289068,1.,0.965925826289068,1.,0.965925826289068,1.,0.965925826289068,
1.,0.965925826289068,1.,0.965925826289068,1.,0.965925826289068,1.,0.965925826289068,
1.,0.965925826289068,1.,0.965925826289068,1.,0.965925826289068,1.,0.965925826289068,
1.,0.965925826289068,1.,0.965925826289068,1.,0.965925826289068,1.,0.965925826289068,
1.,0.965925826289068,1.,0.965925826289068,1.,0.965925826289068,1.,0.965925826289068,
1.,0.965925826289068,1.,0.965925826289068,1.,0.965925826289068,1.,0.965925826289068,
1.,0.965925826289068,1.,0.965925826289068,1.,0.965925826289068,1.,0.965925826289068,
1.,0.965925826289068,1.,0.965925826289068,1.,0.965925826289068,1.,0.965925826289068,
1.,0.965925826289068,1.,0.965925826289068,1.,0.965925826289068,1.,0.965925826289068,
1.,0.965925826289068,1.,0.965925826289068,1.,0.965925826289068,1.,0.965925826289068,
1.,0.965925826289068,1.,0.965925826289068,1.,0.965925826289068,1.)))
REPRESENTATION_ITEM('')
SURFACE()
);
#184=(
BOUNDED_SURFACE()
B_SPLINE_SURFACE(1,2,((#15675,#15676,#15677,#15678,#15679,#15680,#15681,
#15682,#15683,#15684,#15685,#15686,#15687,#15688,#15689,#15690,#15691,#15692,
#15693,#15694,#15695,#15696,#15697,#15698,#15699,#15700,#15701,#15702,#15703,
#15704,#15705,#15706,#15707,#15708,#15709,#15710,#15711,#15712,#15713,#15714,
#15715,#15716,#15717,#15718,#15719,#15720,#15721,#15722,#15723,#15724,#15725,
#15726,#15727,#15728,#15729,#15730,#15731,#15732,#15733,#15734,#15735,#15736,
#15737,#15738,#15739,#15740,#15741,#15742,#15743,#15744,#15745,#15746,#15747,
#15748,#15749,#15750,#15751,#15752,#15753,#15754,#15755,#15756,#15757,#15758,
#15759,#15760,#15761,#15762,#15763,#15764,#15765,#15766,#15767,#15768,#15769,
#15770,#15771,#15772,#15773,#15774,#15775,#15776,#15777,#15778,#15779,#15780,
#15781,#15782,#15783,#15784,#15785,#15786,#15787,#15788,#15789,#15790,#15791,
#15792,#15793,#15794,#15795,#15796,#15797,#15798,#15799,#15800,#15801,#15802,
#15803,#15804,#15805,#15806,#15807,#15808,#15809,#15810,#15811,#15812,#15813,
#15814,#15815,#15816,#15817,#15818,#15819),(#15820,#15821,#15822,#15823,
#15824,#15825,#15826,#15827,#15828,#15829,#15830,#15831,#15832,#15833,#15834,
#15835,#15836,#15837,#15838,#15839,#15840,#15841,#15842,#15843,#15844,#15845,
#15846,#15847,#15848,#15849,#15850,#15851,#15852,#15853,#15854,#15855,#15856,
#15857,#15858,#15859,#15860,#15861,#15862,#15863,#15864,#15865,#15866,#15867,
#15868,#15869,#15870,#15871,#15872,#15873,#15874,#15875,#15876,#15877,#15878,
#15879,#15880,#15881,#15882,#15883,#15884,#15885,#15886,#15887,#15888,#15889,
#15890,#15891,#15892,#15893,#15894,#15895,#15896,#15897,#15898,#15899,#15900,
#15901,#15902,#15903,#15904,#15905,#15906,#15907,#15908,#15909,#15910,#15911,
#15912,#15913,#15914,#15915,#15916,#15917,#15918,#15919,#15920,#15921,#15922,
#15923,#15924,#15925,#15926,#15927,#15928,#15929,#15930,#15931,#15932,#15933,
#15934,#15935,#15936,#15937,#15938,#15939,#15940,#15941,#15942,#15943,#15944,
#15945,#15946,#15947,#15948,#15949,#15950,#15951,#15952,#15953,#15954,#15955,
#15956,#15957,#15958,#15959,#15960,#15961,#15962,#15963,#15964)),
 .UNSPECIFIED.,.F.,.F.,.F.)
B_SPLINE_SURFACE_WITH_KNOTS((2,2),(3,2,2,2,2,2,2,2,2,2,2,2,2,2,2,2,2,2,
2,2,2,2,2,2,2,2,2,2,2,2,2,2,2,2,2,2,2,2,2,2,2,2,2,2,2,2,2,2,2,2,2,2,2,2,
2,2,2,2,2,2,2,2,2,2,2,2,2,2,2,2,2,2,3),(0.,1.),(0.,0.0138888888888889,0.0277777777777778,
0.0416666666666667,0.0555555555555556,0.0694444444444444,0.0833333333333333,
0.0972222222222222,0.111111111111111,0.125,0.138888888888889,0.152777777777778,
0.166666666666667,0.180555555555556,0.194444444444444,0.208333333333333,
0.222222222222222,0.236111111111111,0.25,0.263888888888889,0.277777777777778,
0.291666666666667,0.305555555555556,0.319444444444444,0.333333333333333,
0.347222222222222,0.361111111111111,0.375,0.388888888888889,0.402777777777778,
0.416666666666667,0.430555555555556,0.444444444444444,0.458333333333333,
0.472222222222222,0.486111111111111,0.5,0.513888888888889,0.527777777777778,
0.541666666666667,0.555555555555556,0.569444444444444,0.583333333333333,
0.597222222222222,0.611111111111111,0.625,0.638888888888889,0.652777777777778,
0.666666666666667,0.680555555555556,0.694444444444444,0.708333333333333,
0.722222222222222,0.736111111111111,0.75,0.763888888888889,0.777777777777778,
0.791666666666667,0.805555555555556,0.819444444444444,0.833333333333333,
0.847222222222222,0.861111111111111,0.875,0.888888888888889,0.902777777777778,
0.916666666666667,0.930555555555556,0.944444444444444,0.958333333333333,
0.972222222222222,0.986111111111111,1.),.UNSPECIFIED.)
GEOMETRIC_REPRESENTATION_ITEM()
RATIONAL_B_SPLINE_SURFACE(((1.,0.965925826289068,1.,0.965925826289068,1.,
0.965925826289068,1.,0.965925826289068,1.,0.965925826289068,1.,0.965925826289068,
1.,0.965925826289068,1.,0.965925826289068,1.,0.965925826289068,1.,0.965925826289068,
1.,0.965925826289068,1.,0.965925826289068,1.,0.965925826289068,1.,0.965925826289068,
1.,0.965925826289068,1.,0.965925826289068,1.,0.965925826289068,1.,0.965925826289068,
1.,0.965925826289068,1.,0.965925826289068,1.,0.965925826289068,1.,0.965925826289068,
1.,0.965925826289068,1.,0.965925826289068,1.,0.965925826289068,1.,0.965925826289068,
1.,0.965925826289068,1.,0.965925826289068,1.,0.965925826289068,1.,0.965925826289068,
1.,0.965925826289068,1.,0.965925826289068,1.,0.965925826289068,1.,0.965925826289068,
1.,0.965925826289068,1.,0.965925826289068,1.,0.965925826289068,1.,0.965925826289068,
1.,0.965925826289068,1.,0.965925826289068,1.,0.965925826289068,1.,0.965925826289068,
1.,0.965925826289068,1.,0.965925826289068,1.,0.965925826289068,1.,0.965925826289068,
1.,0.965925826289068,1.,0.965925826289068,1.,0.965925826289068,1.,0.965925826289068,
1.,0.965925826289068,1.,0.965925826289068,1.,0.965925826289068,1.,0.965925826289068,
1.,0.965925826289068,1.,0.965925826289068,1.,0.965925826289068,1.,0.965925826289068,
1.,0.965925826289068,1.,0.965925826289068,1.,0.965925826289068,1.,0.965925826289068,
1.,0.965925826289068,1.,0.965925826289068,1.,0.965925826289068,1.,0.965925826289068,
1.,0.965925826289068,1.,0.965925826289068,1.,0.965925826289068,1.,0.965925826289068,
1.,0.965925826289068,1.,0.965925826289068,1.),(1.,0.965925826289068,1.,
0.965925826289068,1.,0.965925826289068,1.,0.965925826289068,1.,0.965925826289068,
1.,0.965925826289068,1.,0.965925826289068,1.,0.965925826289068,1.,0.965925826289068,
1.,0.965925826289068,1.,0.965925826289068,1.,0.965925826289068,1.,0.965925826289068,
1.,0.965925826289068,1.,0.965925826289068,1.,0.965925826289068,1.,0.965925826289068,
1.,0.965925826289068,1.,0.965925826289068,1.,0.965925826289068,1.,0.965925826289068,
1.,0.965925826289068,1.,0.965925826289068,1.,0.965925826289068,1.,0.965925826289068,
1.,0.965925826289068,1.,0.965925826289068,1.,0.965925826289068,1.,0.965925826289068,
1.,0.965925826289068,1.,0.965925826289068,1.,0.965925826289068,1.,0.965925826289068,
1.,0.965925826289068,1.,0.965925826289068,1.,0.965925826289068,1.,0.965925826289068,
1.,0.965925826289068,1.,0.965925826289068,1.,0.965925826289068,1.,0.965925826289068,
1.,0.965925826289068,1.,0.965925826289068,1.,0.965925826289068,1.,0.965925826289068,
1.,0.965925826289068,1.,0.965925826289068,1.,0.965925826289068,1.,0.965925826289068,
1.,0.965925826289068,1.,0.965925826289068,1.,0.965925826289068,1.,0.965925826289068,
1.,0.965925826289068,1.,0.965925826289068,1.,0.965925826289068,1.,0.965925826289068,
1.,0.965925826289068,1.,0.965925826289068,1.,0.965925826289068,1.,0.965925826289068,
1.,0.965925826289068,1.,0.965925826289068,1.,0.965925826289068,1.,0.965925826289068,
1.,0.965925826289068,1.,0.965925826289068,1.,0.965925826289068,1.,0.965925826289068,
1.,0.965925826289068,1.,0.965925826289068,1.,0.965925826289068,1.)))
REPRESENTATION_ITEM('')
SURFACE()
);
#185=(
BOUNDED_SURFACE()
B_SPLINE_SURFACE(1,2,((#15973,#15974,#15975,#15976,#15977,#15978,#15979,
#15980,#15981,#15982,#15983,#15984,#15985,#15986,#15987,#15988,#15989,#15990,
#15991,#15992,#15993,#15994,#15995,#15996,#15997,#15998,#15999,#16000,#16001,
#16002,#16003,#16004,#16005,#16006,#16007,#16008,#16009,#16010,#16011,#16012,
#16013,#16014,#16015,#16016,#16017,#16018,#16019,#16020,#16021,#16022,#16023,
#16024,#16025,#16026,#16027,#16028,#16029,#16030,#16031,#16032,#16033,#16034,
#16035,#16036,#16037,#16038,#16039,#16040,#16041,#16042,#16043,#16044,#16045,
#16046,#16047,#16048,#16049,#16050,#16051,#16052,#16053,#16054,#16055,#16056,
#16057,#16058,#16059,#16060,#16061,#16062,#16063,#16064,#16065,#16066,#16067,
#16068,#16069,#16070,#16071,#16072,#16073,#16074,#16075,#16076,#16077,#16078,
#16079,#16080,#16081,#16082,#16083,#16084,#16085,#16086,#16087,#16088,#16089,
#16090,#16091,#16092,#16093,#16094,#16095,#16096,#16097,#16098,#16099,#16100,
#16101,#16102,#16103,#16104,#16105,#16106,#16107,#16108,#16109,#16110,#16111,
#16112,#16113,#16114,#16115,#16116,#16117),(#16118,#16119,#16120,#16121,
#16122,#16123,#16124,#16125,#16126,#16127,#16128,#16129,#16130,#16131,#16132,
#16133,#16134,#16135,#16136,#16137,#16138,#16139,#16140,#16141,#16142,#16143,
#16144,#16145,#16146,#16147,#16148,#16149,#16150,#16151,#16152,#16153,#16154,
#16155,#16156,#16157,#16158,#16159,#16160,#16161,#16162,#16163,#16164,#16165,
#16166,#16167,#16168,#16169,#16170,#16171,#16172,#16173,#16174,#16175,#16176,
#16177,#16178,#16179,#16180,#16181,#16182,#16183,#16184,#16185,#16186,#16187,
#16188,#16189,#16190,#16191,#16192,#16193,#16194,#16195,#16196,#16197,#16198,
#16199,#16200,#16201,#16202,#16203,#16204,#16205,#16206,#16207,#16208,#16209,
#16210,#16211,#16212,#16213,#16214,#16215,#16216,#16217,#16218,#16219,#16220,
#16221,#16222,#16223,#16224,#16225,#16226,#16227,#16228,#16229,#16230,#16231,
#16232,#16233,#16234,#16235,#16236,#16237,#16238,#16239,#16240,#16241,#16242,
#16243,#16244,#16245,#16246,#16247,#16248,#16249,#16250,#16251,#16252,#16253,
#16254,#16255,#16256,#16257,#16258,#16259,#16260,#16261,#16262)),
 .UNSPECIFIED.,.F.,.F.,.F.)
B_SPLINE_SURFACE_WITH_KNOTS((2,2),(3,2,2,2,2,2,2,2,2,2,2,2,2,2,2,2,2,2,
2,2,2,2,2,2,2,2,2,2,2,2,2,2,2,2,2,2,2,2,2,2,2,2,2,2,2,2,2,2,2,2,2,2,2,2,
2,2,2,2,2,2,2,2,2,2,2,2,2,2,2,2,2,2,3),(0.,1.),(0.,0.0138888888888889,0.0277777777777778,
0.0416666666666667,0.0555555555555556,0.0694444444444444,0.0833333333333333,
0.0972222222222222,0.111111111111111,0.125,0.138888888888889,0.152777777777778,
0.166666666666667,0.180555555555556,0.194444444444444,0.208333333333333,
0.222222222222222,0.236111111111111,0.25,0.263888888888889,0.277777777777778,
0.291666666666667,0.305555555555556,0.319444444444444,0.333333333333333,
0.347222222222222,0.361111111111111,0.375,0.388888888888889,0.402777777777778,
0.416666666666667,0.430555555555556,0.444444444444444,0.458333333333333,
0.472222222222222,0.486111111111111,0.5,0.513888888888889,0.527777777777778,
0.541666666666667,0.555555555555556,0.569444444444444,0.583333333333333,
0.597222222222222,0.611111111111111,0.625,0.638888888888889,0.652777777777778,
0.666666666666667,0.680555555555556,0.694444444444444,0.708333333333333,
0.722222222222222,0.736111111111111,0.75,0.763888888888889,0.777777777777778,
0.791666666666667,0.805555555555556,0.819444444444444,0.833333333333333,
0.847222222222222,0.861111111111111,0.875,0.888888888888889,0.902777777777778,
0.916666666666667,0.930555555555556,0.944444444444444,0.958333333333333,
0.972222222222222,0.986111111111111,1.),.UNSPECIFIED.)
GEOMETRIC_REPRESENTATION_ITEM()
RATIONAL_B_SPLINE_SURFACE(((1.,0.965925826289068,1.,0.965925826289068,1.,
0.965925826289068,1.,0.965925826289068,1.,0.965925826289068,1.,0.965925826289068,
1.,0.965925826289068,1.,0.965925826289068,1.,0.965925826289068,1.,0.965925826289068,
1.,0.965925826289068,1.,0.965925826289068,1.,0.965925826289068,1.,0.965925826289068,
1.,0.965925826289068,1.,0.965925826289068,1.,0.965925826289068,1.,0.965925826289068,
1.,0.965925826289068,1.,0.965925826289068,1.,0.965925826289068,1.,0.965925826289068,
1.,0.965925826289068,1.,0.965925826289068,1.,0.965925826289068,1.,0.965925826289068,
1.,0.965925826289068,1.,0.965925826289068,1.,0.965925826289068,1.,0.965925826289068,
1.,0.965925826289068,1.,0.965925826289068,1.,0.965925826289068,1.,0.965925826289068,
1.,0.965925826289068,1.,0.965925826289068,1.,0.965925826289068,1.,0.965925826289068,
1.,0.965925826289068,1.,0.965925826289068,1.,0.965925826289068,1.,0.965925826289068,
1.,0.965925826289068,1.,0.965925826289068,1.,0.965925826289068,1.,0.965925826289068,
1.,0.965925826289068,1.,0.965925826289068,1.,0.965925826289068,1.,0.965925826289068,
1.,0.965925826289068,1.,0.965925826289068,1.,0.965925826289068,1.,0.965925826289068,
1.,0.965925826289068,1.,0.965925826289068,1.,0.965925826289068,1.,0.965925826289068,
1.,0.965925826289068,1.,0.965925826289068,1.,0.965925826289068,1.,0.965925826289068,
1.,0.965925826289068,1.,0.965925826289068,1.,0.965925826289068,1.,0.965925826289068,
1.,0.965925826289068,1.,0.965925826289068,1.,0.965925826289068,1.,0.965925826289068,
1.,0.965925826289068,1.,0.965925826289068,1.),(1.,0.965925826289068,1.,
0.965925826289068,1.,0.965925826289068,1.,0.965925826289068,1.,0.965925826289068,
1.,0.965925826289068,1.,0.965925826289068,1.,0.965925826289068,1.,0.965925826289068,
1.,0.965925826289068,1.,0.965925826289068,1.,0.965925826289068,1.,0.965925826289068,
1.,0.965925826289068,1.,0.965925826289068,1.,0.965925826289068,1.,0.965925826289068,
1.,0.965925826289068,1.,0.965925826289068,1.,0.965925826289068,1.,0.965925826289068,
1.,0.965925826289068,1.,0.965925826289068,1.,0.965925826289068,1.,0.965925826289068,
1.,0.965925826289068,1.,0.965925826289068,1.,0.965925826289068,1.,0.965925826289068,
1.,0.965925826289068,1.,0.965925826289068,1.,0.965925826289068,1.,0.965925826289068,
1.,0.965925826289068,1.,0.965925826289068,1.,0.965925826289068,1.,0.965925826289068,
1.,0.965925826289068,1.,0.965925826289068,1.,0.965925826289068,1.,0.965925826289068,
1.,0.965925826289068,1.,0.965925826289068,1.,0.965925826289068,1.,0.965925826289068,
1.,0.965925826289068,1.,0.965925826289068,1.,0.965925826289068,1.,0.965925826289068,
1.,0.965925826289068,1.,0.965925826289068,1.,0.965925826289068,1.,0.965925826289068,
1.,0.965925826289068,1.,0.965925826289068,1.,0.965925826289068,1.,0.965925826289068,
1.,0.965925826289068,1.,0.965925826289068,1.,0.965925826289068,1.,0.965925826289068,
1.,0.965925826289068,1.,0.965925826289068,1.,0.965925826289068,1.,0.965925826289068,
1.,0.965925826289068,1.,0.965925826289068,1.,0.965925826289068,1.,0.965925826289068,
1.,0.965925826289068,1.,0.965925826289068,1.,0.965925826289068,1.)))
REPRESENTATION_ITEM('')
SURFACE()
);
#186=(
BOUNDED_SURFACE()
B_SPLINE_SURFACE(1,2,((#16271,#16272,#16273,#16274,#16275,#16276,#16277,
#16278,#16279,#16280,#16281,#16282,#16283,#16284,#16285,#16286,#16287,#16288,
#16289,#16290,#16291,#16292,#16293,#16294,#16295,#16296,#16297,#16298,#16299,
#16300,#16301,#16302,#16303,#16304,#16305,#16306,#16307,#16308,#16309,#16310,
#16311,#16312,#16313,#16314,#16315,#16316,#16317,#16318,#16319,#16320,#16321,
#16322,#16323,#16324,#16325,#16326,#16327,#16328,#16329,#16330,#16331,#16332,
#16333,#16334,#16335,#16336,#16337,#16338,#16339,#16340,#16341,#16342,#16343,
#16344,#16345,#16346,#16347,#16348,#16349,#16350,#16351,#16352,#16353,#16354,
#16355,#16356,#16357,#16358,#16359,#16360,#16361,#16362,#16363,#16364,#16365,
#16366,#16367,#16368,#16369,#16370,#16371,#16372,#16373,#16374,#16375,#16376,
#16377,#16378,#16379,#16380,#16381,#16382,#16383,#16384,#16385,#16386,#16387,
#16388,#16389,#16390,#16391,#16392,#16393,#16394,#16395,#16396,#16397,#16398,
#16399,#16400,#16401,#16402,#16403,#16404,#16405,#16406,#16407,#16408,#16409,
#16410,#16411,#16412,#16413,#16414,#16415),(#16416,#16417,#16418,#16419,
#16420,#16421,#16422,#16423,#16424,#16425,#16426,#16427,#16428,#16429,#16430,
#16431,#16432,#16433,#16434,#16435,#16436,#16437,#16438,#16439,#16440,#16441,
#16442,#16443,#16444,#16445,#16446,#16447,#16448,#16449,#16450,#16451,#16452,
#16453,#16454,#16455,#16456,#16457,#16458,#16459,#16460,#16461,#16462,#16463,
#16464,#16465,#16466,#16467,#16468,#16469,#16470,#16471,#16472,#16473,#16474,
#16475,#16476,#16477,#16478,#16479,#16480,#16481,#16482,#16483,#16484,#16485,
#16486,#16487,#16488,#16489,#16490,#16491,#16492,#16493,#16494,#16495,#16496,
#16497,#16498,#16499,#16500,#16501,#16502,#16503,#16504,#16505,#16506,#16507,
#16508,#16509,#16510,#16511,#16512,#16513,#16514,#16515,#16516,#16517,#16518,
#16519,#16520,#16521,#16522,#16523,#16524,#16525,#16526,#16527,#16528,#16529,
#16530,#16531,#16532,#16533,#16534,#16535,#16536,#16537,#16538,#16539,#16540,
#16541,#16542,#16543,#16544,#16545,#16546,#16547,#16548,#16549,#16550,#16551,
#16552,#16553,#16554,#16555,#16556,#16557,#16558,#16559,#16560)),
 .UNSPECIFIED.,.F.,.F.,.F.)
B_SPLINE_SURFACE_WITH_KNOTS((2,2),(3,2,2,2,2,2,2,2,2,2,2,2,2,2,2,2,2,2,
2,2,2,2,2,2,2,2,2,2,2,2,2,2,2,2,2,2,2,2,2,2,2,2,2,2,2,2,2,2,2,2,2,2,2,2,
2,2,2,2,2,2,2,2,2,2,2,2,2,2,2,2,2,2,3),(0.,1.),(0.,0.0138888888888889,0.0277777777777778,
0.0416666666666667,0.0555555555555556,0.0694444444444444,0.0833333333333333,
0.0972222222222222,0.111111111111111,0.125,0.138888888888889,0.152777777777778,
0.166666666666667,0.180555555555556,0.194444444444444,0.208333333333333,
0.222222222222222,0.236111111111111,0.25,0.263888888888889,0.277777777777778,
0.291666666666667,0.305555555555556,0.319444444444444,0.333333333333333,
0.347222222222222,0.361111111111111,0.375,0.388888888888889,0.402777777777778,
0.416666666666667,0.430555555555556,0.444444444444444,0.458333333333333,
0.472222222222222,0.486111111111111,0.5,0.513888888888889,0.527777777777778,
0.541666666666667,0.555555555555556,0.569444444444444,0.583333333333333,
0.597222222222222,0.611111111111111,0.625,0.638888888888889,0.652777777777778,
0.666666666666667,0.680555555555556,0.694444444444444,0.708333333333333,
0.722222222222222,0.736111111111111,0.75,0.763888888888889,0.777777777777778,
0.791666666666667,0.805555555555556,0.819444444444444,0.833333333333333,
0.847222222222222,0.861111111111111,0.875,0.888888888888889,0.902777777777778,
0.916666666666667,0.930555555555556,0.944444444444444,0.958333333333333,
0.972222222222222,0.986111111111111,1.),.UNSPECIFIED.)
GEOMETRIC_REPRESENTATION_ITEM()
RATIONAL_B_SPLINE_SURFACE(((1.,0.965925826289068,1.,0.965925826289068,1.,
0.965925826289068,1.,0.965925826289068,1.,0.965925826289068,1.,0.965925826289068,
1.,0.965925826289068,1.,0.965925826289068,1.,0.965925826289068,1.,0.965925826289068,
1.,0.965925826289068,1.,0.965925826289068,1.,0.965925826289068,1.,0.965925826289068,
1.,0.965925826289068,1.,0.965925826289068,1.,0.965925826289068,1.,0.965925826289068,
1.,0.965925826289068,1.,0.965925826289068,1.,0.965925826289068,1.,0.965925826289068,
1.,0.965925826289068,1.,0.965925826289068,1.,0.965925826289068,1.,0.965925826289068,
1.,0.965925826289068,1.,0.965925826289068,1.,0.965925826289068,1.,0.965925826289068,
1.,0.965925826289068,1.,0.965925826289068,1.,0.965925826289068,1.,0.965925826289068,
1.,0.965925826289068,1.,0.965925826289068,1.,0.965925826289068,1.,0.965925826289068,
1.,0.965925826289068,1.,0.965925826289068,1.,0.965925826289068,1.,0.965925826289068,
1.,0.965925826289068,1.,0.965925826289068,1.,0.965925826289068,1.,0.965925826289068,
1.,0.965925826289068,1.,0.965925826289068,1.,0.965925826289068,1.,0.965925826289068,
1.,0.965925826289068,1.,0.965925826289068,1.,0.965925826289068,1.,0.965925826289068,
1.,0.965925826289068,1.,0.965925826289068,1.,0.965925826289068,1.,0.965925826289068,
1.,0.965925826289068,1.,0.965925826289068,1.,0.965925826289068,1.,0.965925826289068,
1.,0.965925826289068,1.,0.965925826289068,1.,0.965925826289068,1.,0.965925826289068,
1.,0.965925826289068,1.,0.965925826289068,1.,0.965925826289068,1.,0.965925826289068,
1.,0.965925826289068,1.,0.965925826289068,1.),(1.,0.965925826289068,1.,
0.965925826289068,1.,0.965925826289068,1.,0.965925826289068,1.,0.965925826289068,
1.,0.965925826289068,1.,0.965925826289068,1.,0.965925826289068,1.,0.965925826289068,
1.,0.965925826289068,1.,0.965925826289068,1.,0.965925826289068,1.,0.965925826289068,
1.,0.965925826289068,1.,0.965925826289068,1.,0.965925826289068,1.,0.965925826289068,
1.,0.965925826289068,1.,0.965925826289068,1.,0.965925826289068,1.,0.965925826289068,
1.,0.965925826289068,1.,0.965925826289068,1.,0.965925826289068,1.,0.965925826289068,
1.,0.965925826289068,1.,0.965925826289068,1.,0.965925826289068,1.,0.965925826289068,
1.,0.965925826289068,1.,0.965925826289068,1.,0.965925826289068,1.,0.965925826289068,
1.,0.965925826289068,1.,0.965925826289068,1.,0.965925826289068,1.,0.965925826289068,
1.,0.965925826289068,1.,0.965925826289068,1.,0.965925826289068,1.,0.965925826289068,
1.,0.965925826289068,1.,0.965925826289068,1.,0.965925826289068,1.,0.965925826289068,
1.,0.965925826289068,1.,0.965925826289068,1.,0.965925826289068,1.,0.965925826289068,
1.,0.965925826289068,1.,0.965925826289068,1.,0.965925826289068,1.,0.965925826289068,
1.,0.965925826289068,1.,0.965925826289068,1.,0.965925826289068,1.,0.965925826289068,
1.,0.965925826289068,1.,0.965925826289068,1.,0.965925826289068,1.,0.965925826289068,
1.,0.965925826289068,1.,0.965925826289068,1.,0.965925826289068,1.,0.965925826289068,
1.,0.965925826289068,1.,0.965925826289068,1.,0.965925826289068,1.,0.965925826289068,
1.,0.965925826289068,1.,0.965925826289068,1.,0.965925826289068,1.)))
REPRESENTATION_ITEM('')
SURFACE()
);
#187=(
BOUNDED_SURFACE()
B_SPLINE_SURFACE(1,2,((#16577,#16578,#16579,#16580,#16581,#16582,#16583,
#16584,#16585,#16586,#16587,#16588,#16589,#16590,#16591,#16592,#16593,#16594,
#16595,#16596,#16597,#16598,#16599,#16600,#16601,#16602,#16603,#16604,#16605,
#16606,#16607,#16608,#16609,#16610,#16611,#16612,#16613,#16614,#16615,#16616,
#16617,#16618,#16619,#16620,#16621,#16622,#16623,#16624,#16625,#16626,#16627,
#16628,#16629,#16630,#16631,#16632,#16633,#16634,#16635,#16636,#16637,#16638,
#16639,#16640,#16641,#16642,#16643,#16644,#16645,#16646,#16647,#16648,#16649,
#16650,#16651,#16652,#16653,#16654,#16655,#16656,#16657,#16658,#16659,#16660,
#16661,#16662,#16663,#16664,#16665,#16666,#16667,#16668,#16669,#16670,#16671,
#16672,#16673,#16674,#16675,#16676,#16677,#16678,#16679,#16680,#16681,#16682,
#16683,#16684,#16685,#16686,#16687,#16688,#16689,#16690,#16691,#16692,#16693,
#16694,#16695,#16696,#16697,#16698,#16699,#16700,#16701,#16702,#16703,#16704,
#16705,#16706,#16707,#16708,#16709,#16710,#16711,#16712,#16713,#16714,#16715,
#16716,#16717,#16718,#16719,#16720,#16721),(#16722,#16723,#16724,#16725,
#16726,#16727,#16728,#16729,#16730,#16731,#16732,#16733,#16734,#16735,#16736,
#16737,#16738,#16739,#16740,#16741,#16742,#16743,#16744,#16745,#16746,#16747,
#16748,#16749,#16750,#16751,#16752,#16753,#16754,#16755,#16756,#16757,#16758,
#16759,#16760,#16761,#16762,#16763,#16764,#16765,#16766,#16767,#16768,#16769,
#16770,#16771,#16772,#16773,#16774,#16775,#16776,#16777,#16778,#16779,#16780,
#16781,#16782,#16783,#16784,#16785,#16786,#16787,#16788,#16789,#16790,#16791,
#16792,#16793,#16794,#16795,#16796,#16797,#16798,#16799,#16800,#16801,#16802,
#16803,#16804,#16805,#16806,#16807,#16808,#16809,#16810,#16811,#16812,#16813,
#16814,#16815,#16816,#16817,#16818,#16819,#16820,#16821,#16822,#16823,#16824,
#16825,#16826,#16827,#16828,#16829,#16830,#16831,#16832,#16833,#16834,#16835,
#16836,#16837,#16838,#16839,#16840,#16841,#16842,#16843,#16844,#16845,#16846,
#16847,#16848,#16849,#16850,#16851,#16852,#16853,#16854,#16855,#16856,#16857,
#16858,#16859,#16860,#16861,#16862,#16863,#16864,#16865,#16866)),
 .UNSPECIFIED.,.F.,.F.,.F.)
B_SPLINE_SURFACE_WITH_KNOTS((2,2),(3,2,2,2,2,2,2,2,2,2,2,2,2,2,2,2,2,2,
2,2,2,2,2,2,2,2,2,2,2,2,2,2,2,2,2,2,2,2,2,2,2,2,2,2,2,2,2,2,2,2,2,2,2,2,
2,2,2,2,2,2,2,2,2,2,2,2,2,2,2,2,2,2,3),(0.,1.),(0.,0.0138888888888889,0.0277777777777778,
0.0416666666666667,0.0555555555555556,0.0694444444444444,0.0833333333333333,
0.0972222222222222,0.111111111111111,0.125,0.138888888888889,0.152777777777778,
0.166666666666667,0.180555555555556,0.194444444444444,0.208333333333333,
0.222222222222222,0.236111111111111,0.25,0.263888888888889,0.277777777777778,
0.291666666666667,0.305555555555556,0.319444444444444,0.333333333333333,
0.347222222222222,0.361111111111111,0.375,0.388888888888889,0.402777777777778,
0.416666666666667,0.430555555555556,0.444444444444444,0.458333333333333,
0.472222222222222,0.486111111111111,0.5,0.513888888888889,0.527777777777778,
0.541666666666667,0.555555555555556,0.569444444444444,0.583333333333333,
0.597222222222222,0.611111111111111,0.625,0.638888888888889,0.652777777777778,
0.666666666666667,0.680555555555556,0.694444444444444,0.708333333333333,
0.722222222222222,0.736111111111111,0.75,0.763888888888889,0.777777777777778,
0.791666666666667,0.805555555555556,0.819444444444444,0.833333333333333,
0.847222222222222,0.861111111111111,0.875,0.888888888888889,0.902777777777778,
0.916666666666667,0.930555555555556,0.944444444444444,0.958333333333333,
0.972222222222222,0.986111111111111,1.),.UNSPECIFIED.)
GEOMETRIC_REPRESENTATION_ITEM()
RATIONAL_B_SPLINE_SURFACE(((1.,0.965925826289068,1.,0.965925826289068,1.,
0.965925826289068,1.,0.965925826289068,1.,0.965925826289068,1.,0.965925826289068,
1.,0.965925826289068,1.,0.965925826289068,1.,0.965925826289068,1.,0.965925826289068,
1.,0.965925826289068,1.,0.965925826289068,1.,0.965925826289068,1.,0.965925826289068,
1.,0.965925826289068,1.,0.965925826289068,1.,0.965925826289068,1.,0.965925826289068,
1.,0.965925826289068,1.,0.965925826289068,1.,0.965925826289068,1.,0.965925826289068,
1.,0.965925826289068,1.,0.965925826289068,1.,0.965925826289068,1.,0.965925826289068,
1.,0.965925826289068,1.,0.965925826289068,1.,0.965925826289068,1.,0.965925826289068,
1.,0.965925826289068,1.,0.965925826289068,1.,0.965925826289068,1.,0.965925826289068,
1.,0.965925826289068,1.,0.965925826289068,1.,0.965925826289068,1.,0.965925826289068,
1.,0.965925826289068,1.,0.965925826289068,1.,0.965925826289068,1.,0.965925826289068,
1.,0.965925826289068,1.,0.965925826289068,1.,0.965925826289068,1.,0.965925826289068,
1.,0.965925826289068,1.,0.965925826289068,1.,0.965925826289068,1.,0.965925826289068,
1.,0.965925826289068,1.,0.965925826289068,1.,0.965925826289068,1.,0.965925826289068,
1.,0.965925826289068,1.,0.965925826289068,1.,0.965925826289068,1.,0.965925826289068,
1.,0.965925826289068,1.,0.965925826289068,1.,0.965925826289068,1.,0.965925826289068,
1.,0.965925826289068,1.,0.965925826289068,1.,0.965925826289068,1.,0.965925826289068,
1.,0.965925826289068,1.,0.965925826289068,1.,0.965925826289068,1.,0.965925826289068,
1.,0.965925826289068,1.,0.965925826289068,1.),(1.,0.965925826289068,1.,
0.965925826289068,1.,0.965925826289068,1.,0.965925826289068,1.,0.965925826289068,
1.,0.965925826289068,1.,0.965925826289068,1.,0.965925826289068,1.,0.965925826289068,
1.,0.965925826289068,1.,0.965925826289068,1.,0.965925826289068,1.,0.965925826289068,
1.,0.965925826289068,1.,0.965925826289068,1.,0.965925826289068,1.,0.965925826289068,
1.,0.965925826289068,1.,0.965925826289068,1.,0.965925826289068,1.,0.965925826289068,
1.,0.965925826289068,1.,0.965925826289068,1.,0.965925826289068,1.,0.965925826289068,
1.,0.965925826289068,1.,0.965925826289068,1.,0.965925826289068,1.,0.965925826289068,
1.,0.965925826289068,1.,0.965925826289068,1.,0.965925826289068,1.,0.965925826289068,
1.,0.965925826289068,1.,0.965925826289068,1.,0.965925826289068,1.,0.965925826289068,
1.,0.965925826289068,1.,0.965925826289068,1.,0.965925826289068,1.,0.965925826289068,
1.,0.965925826289068,1.,0.965925826289068,1.,0.965925826289068,1.,0.965925826289068,
1.,0.965925826289068,1.,0.965925826289068,1.,0.965925826289068,1.,0.965925826289068,
1.,0.965925826289068,1.,0.965925826289068,1.,0.965925826289068,1.,0.965925826289068,
1.,0.965925826289068,1.,0.965925826289068,1.,0.965925826289068,1.,0.965925826289068,
1.,0.965925826289068,1.,0.965925826289068,1.,0.965925826289068,1.,0.965925826289068,
1.,0.965925826289068,1.,0.965925826289068,1.,0.965925826289068,1.,0.965925826289068,
1.,0.965925826289068,1.,0.965925826289068,1.,0.965925826289068,1.,0.965925826289068,
1.,0.965925826289068,1.,0.965925826289068,1.,0.965925826289068,1.)))
REPRESENTATION_ITEM('')
SURFACE()
);
#188=(
BOUNDED_SURFACE()
B_SPLINE_SURFACE(1,2,((#17011,#17012,#17013,#17014,#17015,#17016,#17017,
#17018,#17019,#17020,#17021,#17022,#17023,#17024,#17025,#17026,#17027,#17028,
#17029,#17030,#17031,#17032,#17033,#17034,#17035,#17036,#17037,#17038,#17039,
#17040,#17041,#17042,#17043,#17044,#17045,#17046,#17047,#17048,#17049,#17050,
#17051,#17052,#17053,#17054,#17055,#17056,#17057,#17058,#17059,#17060,#17061,
#17062,#17063,#17064,#17065,#17066,#17067,#17068,#17069,#17070,#17071,#17072,
#17073,#17074,#17075,#17076,#17077,#17078,#17079,#17080,#17081,#17082,#17083,
#17084,#17085,#17086,#17087,#17088,#17089,#17090,#17091,#17092,#17093,#17094,
#17095,#17096,#17097,#17098,#17099,#17100,#17101,#17102,#17103,#17104,#17105,
#17106,#17107,#17108,#17109,#17110,#17111,#17112,#17113,#17114,#17115,#17116,
#17117,#17118,#17119,#17120,#17121,#17122,#17123,#17124,#17125,#17126,#17127,
#17128,#17129,#17130,#17131,#17132,#17133,#17134,#17135,#17136,#17137,#17138,
#17139,#17140,#17141,#17142,#17143,#17144,#17145,#17146,#17147,#17148,#17149,
#17150,#17151,#17152,#17153,#17154,#17155),(#17156,#17157,#17158,#17159,
#17160,#17161,#17162,#17163,#17164,#17165,#17166,#17167,#17168,#17169,#17170,
#17171,#17172,#17173,#17174,#17175,#17176,#17177,#17178,#17179,#17180,#17181,
#17182,#17183,#17184,#17185,#17186,#17187,#17188,#17189,#17190,#17191,#17192,
#17193,#17194,#17195,#17196,#17197,#17198,#17199,#17200,#17201,#17202,#17203,
#17204,#17205,#17206,#17207,#17208,#17209,#17210,#17211,#17212,#17213,#17214,
#17215,#17216,#17217,#17218,#17219,#17220,#17221,#17222,#17223,#17224,#17225,
#17226,#17227,#17228,#17229,#17230,#17231,#17232,#17233,#17234,#17235,#17236,
#17237,#17238,#17239,#17240,#17241,#17242,#17243,#17244,#17245,#17246,#17247,
#17248,#17249,#17250,#17251,#17252,#17253,#17254,#17255,#17256,#17257,#17258,
#17259,#17260,#17261,#17262,#17263,#17264,#17265,#17266,#17267,#17268,#17269,
#17270,#17271,#17272,#17273,#17274,#17275,#17276,#17277,#17278,#17279,#17280,
#17281,#17282,#17283,#17284,#17285,#17286,#17287,#17288,#17289,#17290,#17291,
#17292,#17293,#17294,#17295,#17296,#17297,#17298,#17299,#17300)),
 .UNSPECIFIED.,.F.,.F.,.F.)
B_SPLINE_SURFACE_WITH_KNOTS((2,2),(3,2,2,2,2,2,2,2,2,2,2,2,2,2,2,2,2,2,
2,2,2,2,2,2,2,2,2,2,2,2,2,2,2,2,2,2,2,2,2,2,2,2,2,2,2,2,2,2,2,2,2,2,2,2,
2,2,2,2,2,2,2,2,2,2,2,2,2,2,2,2,2,2,3),(0.,1.),(0.,0.0138888888888889,0.0277777777777778,
0.0416666666666667,0.0555555555555556,0.0694444444444444,0.0833333333333333,
0.0972222222222222,0.111111111111111,0.125,0.138888888888889,0.152777777777778,
0.166666666666667,0.180555555555556,0.194444444444444,0.208333333333333,
0.222222222222222,0.236111111111111,0.25,0.263888888888889,0.277777777777778,
0.291666666666667,0.305555555555556,0.319444444444444,0.333333333333333,
0.347222222222222,0.361111111111111,0.375,0.388888888888889,0.402777777777778,
0.416666666666667,0.430555555555556,0.444444444444444,0.458333333333333,
0.472222222222222,0.486111111111111,0.5,0.513888888888889,0.527777777777778,
0.541666666666667,0.555555555555556,0.569444444444444,0.583333333333333,
0.597222222222222,0.611111111111111,0.625,0.638888888888889,0.652777777777778,
0.666666666666667,0.680555555555556,0.694444444444444,0.708333333333333,
0.722222222222222,0.736111111111111,0.75,0.763888888888889,0.777777777777778,
0.791666666666667,0.805555555555556,0.819444444444444,0.833333333333333,
0.847222222222222,0.861111111111111,0.875,0.888888888888889,0.902777777777778,
0.916666666666667,0.930555555555556,0.944444444444444,0.958333333333333,
0.972222222222222,0.986111111111111,1.),.UNSPECIFIED.)
GEOMETRIC_REPRESENTATION_ITEM()
RATIONAL_B_SPLINE_SURFACE(((1.,0.965925826289068,1.,0.965925826289068,1.,
0.965925826289068,1.,0.965925826289068,1.,0.965925826289068,1.,0.965925826289068,
1.,0.965925826289068,1.,0.965925826289068,1.,0.965925826289068,1.,0.965925826289068,
1.,0.965925826289068,1.,0.965925826289068,1.,0.965925826289068,1.,0.965925826289068,
1.,0.965925826289068,1.,0.965925826289068,1.,0.965925826289068,1.,0.965925826289068,
1.,0.965925826289068,1.,0.965925826289068,1.,0.965925826289068,1.,0.965925826289068,
1.,0.965925826289068,1.,0.965925826289068,1.,0.965925826289068,1.,0.965925826289068,
1.,0.965925826289068,1.,0.965925826289068,1.,0.965925826289068,1.,0.965925826289068,
1.,0.965925826289068,1.,0.965925826289068,1.,0.965925826289068,1.,0.965925826289068,
1.,0.965925826289068,1.,0.965925826289068,1.,0.965925826289068,1.,0.965925826289068,
1.,0.965925826289068,1.,0.965925826289068,1.,0.965925826289068,1.,0.965925826289068,
1.,0.965925826289068,1.,0.965925826289068,1.,0.965925826289068,1.,0.965925826289068,
1.,0.965925826289068,1.,0.965925826289068,1.,0.965925826289068,1.,0.965925826289068,
1.,0.965925826289068,1.,0.965925826289068,1.,0.965925826289068,1.,0.965925826289068,
1.,0.965925826289068,1.,0.965925826289068,1.,0.965925826289068,1.,0.965925826289068,
1.,0.965925826289068,1.,0.965925826289068,1.,0.965925826289068,1.,0.965925826289068,
1.,0.965925826289068,1.,0.965925826289068,1.,0.965925826289068,1.,0.965925826289068,
1.,0.965925826289068,1.,0.965925826289068,1.,0.965925826289068,1.,0.965925826289068,
1.,0.965925826289068,1.,0.965925826289068,1.),(1.,0.965925826289068,1.,
0.965925826289068,1.,0.965925826289068,1.,0.965925826289068,1.,0.965925826289068,
1.,0.965925826289068,1.,0.965925826289068,1.,0.965925826289068,1.,0.965925826289068,
1.,0.965925826289068,1.,0.965925826289068,1.,0.965925826289068,1.,0.965925826289068,
1.,0.965925826289068,1.,0.965925826289068,1.,0.965925826289068,1.,0.965925826289068,
1.,0.965925826289068,1.,0.965925826289068,1.,0.965925826289068,1.,0.965925826289068,
1.,0.965925826289068,1.,0.965925826289068,1.,0.965925826289068,1.,0.965925826289068,
1.,0.965925826289068,1.,0.965925826289068,1.,0.965925826289068,1.,0.965925826289068,
1.,0.965925826289068,1.,0.965925826289068,1.,0.965925826289068,1.,0.965925826289068,
1.,0.965925826289068,1.,0.965925826289068,1.,0.965925826289068,1.,0.965925826289068,
1.,0.965925826289068,1.,0.965925826289068,1.,0.965925826289068,1.,0.965925826289068,
1.,0.965925826289068,1.,0.965925826289068,1.,0.965925826289068,1.,0.965925826289068,
1.,0.965925826289068,1.,0.965925826289068,1.,0.965925826289068,1.,0.965925826289068,
1.,0.965925826289068,1.,0.965925826289068,1.,0.965925826289068,1.,0.965925826289068,
1.,0.965925826289068,1.,0.965925826289068,1.,0.965925826289068,1.,0.965925826289068,
1.,0.965925826289068,1.,0.965925826289068,1.,0.965925826289068,1.,0.965925826289068,
1.,0.965925826289068,1.,0.965925826289068,1.,0.965925826289068,1.,0.965925826289068,
1.,0.965925826289068,1.,0.965925826289068,1.,0.965925826289068,1.,0.965925826289068,
1.,0.965925826289068,1.,0.965925826289068,1.,0.965925826289068,1.)))
REPRESENTATION_ITEM('')
SURFACE()
);
#189=(
BOUNDED_SURFACE()
B_SPLINE_SURFACE(1,2,((#17308,#17309,#17310,#17311,#17312,#17313,#17314,
#17315,#17316,#17317,#17318,#17319,#17320,#17321,#17322,#17323,#17324,#17325,
#17326,#17327,#17328,#17329,#17330,#17331,#17332,#17333,#17334,#17335,#17336,
#17337,#17338,#17339,#17340,#17341,#17342,#17343,#17344,#17345,#17346,#17347,
#17348,#17349,#17350,#17351,#17352,#17353,#17354,#17355,#17356,#17357,#17358,
#17359,#17360,#17361,#17362,#17363,#17364,#17365,#17366,#17367,#17368,#17369,
#17370,#17371,#17372,#17373,#17374,#17375,#17376,#17377,#17378,#17379,#17380,
#17381,#17382,#17383,#17384,#17385,#17386,#17387,#17388,#17389,#17390,#17391,
#17392,#17393,#17394,#17395,#17396,#17397,#17398,#17399,#17400,#17401,#17402,
#17403,#17404,#17405,#17406,#17407,#17408,#17409,#17410,#17411,#17412,#17413,
#17414,#17415,#17416,#17417,#17418,#17419,#17420,#17421,#17422,#17423,#17424,
#17425,#17426,#17427,#17428,#17429,#17430,#17431,#17432,#17433,#17434,#17435,
#17436,#17437,#17438,#17439,#17440,#17441,#17442,#17443,#17444,#17445,#17446,
#17447,#17448,#17449,#17450,#17451,#17452),(#17453,#17454,#17455,#17456,
#17457,#17458,#17459,#17460,#17461,#17462,#17463,#17464,#17465,#17466,#17467,
#17468,#17469,#17470,#17471,#17472,#17473,#17474,#17475,#17476,#17477,#17478,
#17479,#17480,#17481,#17482,#17483,#17484,#17485,#17486,#17487,#17488,#17489,
#17490,#17491,#17492,#17493,#17494,#17495,#17496,#17497,#17498,#17499,#17500,
#17501,#17502,#17503,#17504,#17505,#17506,#17507,#17508,#17509,#17510,#17511,
#17512,#17513,#17514,#17515,#17516,#17517,#17518,#17519,#17520,#17521,#17522,
#17523,#17524,#17525,#17526,#17527,#17528,#17529,#17530,#17531,#17532,#17533,
#17534,#17535,#17536,#17537,#17538,#17539,#17540,#17541,#17542,#17543,#17544,
#17545,#17546,#17547,#17548,#17549,#17550,#17551,#17552,#17553,#17554,#17555,
#17556,#17557,#17558,#17559,#17560,#17561,#17562,#17563,#17564,#17565,#17566,
#17567,#17568,#17569,#17570,#17571,#17572,#17573,#17574,#17575,#17576,#17577,
#17578,#17579,#17580,#17581,#17582,#17583,#17584,#17585,#17586,#17587,#17588,
#17589,#17590,#17591,#17592,#17593,#17594,#17595,#17596,#17597)),
 .UNSPECIFIED.,.F.,.F.,.F.)
B_SPLINE_SURFACE_WITH_KNOTS((2,2),(3,2,2,2,2,2,2,2,2,2,2,2,2,2,2,2,2,2,
2,2,2,2,2,2,2,2,2,2,2,2,2,2,2,2,2,2,2,2,2,2,2,2,2,2,2,2,2,2,2,2,2,2,2,2,
2,2,2,2,2,2,2,2,2,2,2,2,2,2,2,2,2,2,3),(0.,1.),(0.,0.0138888888888889,0.0277777777777778,
0.0416666666666667,0.0555555555555556,0.0694444444444444,0.0833333333333333,
0.0972222222222222,0.111111111111111,0.125,0.138888888888889,0.152777777777778,
0.166666666666667,0.180555555555556,0.194444444444444,0.208333333333333,
0.222222222222222,0.236111111111111,0.25,0.263888888888889,0.277777777777778,
0.291666666666667,0.305555555555556,0.319444444444444,0.333333333333333,
0.347222222222222,0.361111111111111,0.375,0.388888888888889,0.402777777777778,
0.416666666666667,0.430555555555556,0.444444444444444,0.458333333333333,
0.472222222222222,0.486111111111111,0.5,0.513888888888889,0.527777777777778,
0.541666666666667,0.555555555555556,0.569444444444444,0.583333333333333,
0.597222222222222,0.611111111111111,0.625,0.638888888888889,0.652777777777778,
0.666666666666667,0.680555555555556,0.694444444444444,0.708333333333333,
0.722222222222222,0.736111111111111,0.75,0.763888888888889,0.777777777777778,
0.791666666666667,0.805555555555556,0.819444444444444,0.833333333333333,
0.847222222222222,0.861111111111111,0.875,0.888888888888889,0.902777777777778,
0.916666666666667,0.930555555555556,0.944444444444444,0.958333333333333,
0.972222222222222,0.986111111111111,1.),.UNSPECIFIED.)
GEOMETRIC_REPRESENTATION_ITEM()
RATIONAL_B_SPLINE_SURFACE(((1.,0.965925826289068,1.,0.965925826289068,1.,
0.965925826289068,1.,0.965925826289068,1.,0.965925826289068,1.,0.965925826289068,
1.,0.965925826289068,1.,0.965925826289068,1.,0.965925826289068,1.,0.965925826289068,
1.,0.965925826289068,1.,0.965925826289068,1.,0.965925826289068,1.,0.965925826289068,
1.,0.965925826289068,1.,0.965925826289068,1.,0.965925826289068,1.,0.965925826289068,
1.,0.965925826289068,1.,0.965925826289068,1.,0.965925826289068,1.,0.965925826289068,
1.,0.965925826289068,1.,0.965925826289068,1.,0.965925826289068,1.,0.965925826289068,
1.,0.965925826289068,1.,0.965925826289068,1.,0.965925826289068,1.,0.965925826289068,
1.,0.965925826289068,1.,0.965925826289068,1.,0.965925826289068,1.,0.965925826289068,
1.,0.965925826289068,1.,0.965925826289068,1.,0.965925826289068,1.,0.965925826289068,
1.,0.965925826289068,1.,0.965925826289068,1.,0.965925826289068,1.,0.965925826289068,
1.,0.965925826289068,1.,0.965925826289068,1.,0.965925826289068,1.,0.965925826289068,
1.,0.965925826289068,1.,0.965925826289068,1.,0.965925826289068,1.,0.965925826289068,
1.,0.965925826289068,1.,0.965925826289068,1.,0.965925826289068,1.,0.965925826289068,
1.,0.965925826289068,1.,0.965925826289068,1.,0.965925826289068,1.,0.965925826289068,
1.,0.965925826289068,1.,0.965925826289068,1.,0.965925826289068,1.,0.965925826289068,
1.,0.965925826289068,1.,0.965925826289068,1.,0.965925826289068,1.,0.965925826289068,
1.,0.965925826289068,1.,0.965925826289068,1.,0.965925826289068,1.,0.965925826289068,
1.,0.965925826289068,1.,0.965925826289068,1.),(1.,0.965925826289068,1.,
0.965925826289068,1.,0.965925826289068,1.,0.965925826289068,1.,0.965925826289068,
1.,0.965925826289068,1.,0.965925826289068,1.,0.965925826289068,1.,0.965925826289068,
1.,0.965925826289068,1.,0.965925826289068,1.,0.965925826289068,1.,0.965925826289068,
1.,0.965925826289068,1.,0.965925826289068,1.,0.965925826289068,1.,0.965925826289068,
1.,0.965925826289068,1.,0.965925826289068,1.,0.965925826289068,1.,0.965925826289068,
1.,0.965925826289068,1.,0.965925826289068,1.,0.965925826289068,1.,0.965925826289068,
1.,0.965925826289068,1.,0.965925826289068,1.,0.965925826289068,1.,0.965925826289068,
1.,0.965925826289068,1.,0.965925826289068,1.,0.965925826289068,1.,0.965925826289068,
1.,0.965925826289068,1.,0.965925826289068,1.,0.965925826289068,1.,0.965925826289068,
1.,0.965925826289068,1.,0.965925826289068,1.,0.965925826289068,1.,0.965925826289068,
1.,0.965925826289068,1.,0.965925826289068,1.,0.965925826289068,1.,0.965925826289068,
1.,0.965925826289068,1.,0.965925826289068,1.,0.965925826289068,1.,0.965925826289068,
1.,0.965925826289068,1.,0.965925826289068,1.,0.965925826289068,1.,0.965925826289068,
1.,0.965925826289068,1.,0.965925826289068,1.,0.965925826289068,1.,0.965925826289068,
1.,0.965925826289068,1.,0.965925826289068,1.,0.965925826289068,1.,0.965925826289068,
1.,0.965925826289068,1.,0.965925826289068,1.,0.965925826289068,1.,0.965925826289068,
1.,0.965925826289068,1.,0.965925826289068,1.,0.965925826289068,1.,0.965925826289068,
1.,0.965925826289068,1.,0.965925826289068,1.,0.965925826289068,1.)))
REPRESENTATION_ITEM('')
SURFACE()
);
#190=(
BOUNDED_SURFACE()
B_SPLINE_SURFACE(1,2,((#17653,#17654,#17655,#17656,#17657,#17658,#17659,
#17660,#17661,#17662,#17663,#17664,#17665,#17666,#17667,#17668,#17669,#17670,
#17671,#17672,#17673,#17674,#17675,#17676,#17677,#17678,#17679,#17680,#17681,
#17682,#17683,#17684,#17685,#17686,#17687,#17688,#17689,#17690,#17691,#17692,
#17693,#17694,#17695,#17696,#17697,#17698,#17699,#17700,#17701,#17702,#17703,
#17704,#17705,#17706,#17707,#17708,#17709,#17710,#17711,#17712,#17713,#17714,
#17715,#17716,#17717,#17718,#17719,#17720,#17721,#17722,#17723,#17724,#17725,
#17726,#17727,#17728,#17729,#17730,#17731,#17732,#17733,#17734,#17735,#17736,
#17737,#17738,#17739,#17740,#17741,#17742,#17743,#17744,#17745,#17746,#17747,
#17748,#17749,#17750,#17751,#17752,#17753,#17754,#17755,#17756,#17757,#17758,
#17759,#17760,#17761,#17762,#17763,#17764,#17765,#17766,#17767,#17768,#17769,
#17770,#17771,#17772,#17773,#17774,#17775,#17776,#17777,#17778,#17779,#17780,
#17781,#17782,#17783,#17784,#17785,#17786,#17787,#17788,#17789,#17790,#17791,
#17792,#17793,#17794,#17795,#17796,#17797),(#17798,#17799,#17800,#17801,
#17802,#17803,#17804,#17805,#17806,#17807,#17808,#17809,#17810,#17811,#17812,
#17813,#17814,#17815,#17816,#17817,#17818,#17819,#17820,#17821,#17822,#17823,
#17824,#17825,#17826,#17827,#17828,#17829,#17830,#17831,#17832,#17833,#17834,
#17835,#17836,#17837,#17838,#17839,#17840,#17841,#17842,#17843,#17844,#17845,
#17846,#17847,#17848,#17849,#17850,#17851,#17852,#17853,#17854,#17855,#17856,
#17857,#17858,#17859,#17860,#17861,#17862,#17863,#17864,#17865,#17866,#17867,
#17868,#17869,#17870,#17871,#17872,#17873,#17874,#17875,#17876,#17877,#17878,
#17879,#17880,#17881,#17882,#17883,#17884,#17885,#17886,#17887,#17888,#17889,
#17890,#17891,#17892,#17893,#17894,#17895,#17896,#17897,#17898,#17899,#17900,
#17901,#17902,#17903,#17904,#17905,#17906,#17907,#17908,#17909,#17910,#17911,
#17912,#17913,#17914,#17915,#17916,#17917,#17918,#17919,#17920,#17921,#17922,
#17923,#17924,#17925,#17926,#17927,#17928,#17929,#17930,#17931,#17932,#17933,
#17934,#17935,#17936,#17937,#17938,#17939,#17940,#17941,#17942)),
 .UNSPECIFIED.,.F.,.F.,.F.)
B_SPLINE_SURFACE_WITH_KNOTS((2,2),(3,2,2,2,2,2,2,2,2,2,2,2,2,2,2,2,2,2,
2,2,2,2,2,2,2,2,2,2,2,2,2,2,2,2,2,2,2,2,2,2,2,2,2,2,2,2,2,2,2,2,2,2,2,2,
2,2,2,2,2,2,2,2,2,2,2,2,2,2,2,2,2,2,3),(0.,1.),(0.,0.0138888888888889,0.0277777777777778,
0.0416666666666667,0.0555555555555556,0.0694444444444444,0.0833333333333333,
0.0972222222222222,0.111111111111111,0.125,0.138888888888889,0.152777777777778,
0.166666666666667,0.180555555555556,0.194444444444444,0.208333333333333,
0.222222222222222,0.236111111111111,0.25,0.263888888888889,0.277777777777778,
0.291666666666667,0.305555555555556,0.319444444444444,0.333333333333333,
0.347222222222222,0.361111111111111,0.375,0.388888888888889,0.402777777777778,
0.416666666666667,0.430555555555556,0.444444444444444,0.458333333333333,
0.472222222222222,0.486111111111111,0.5,0.513888888888889,0.527777777777778,
0.541666666666667,0.555555555555556,0.569444444444444,0.583333333333333,
0.597222222222222,0.611111111111111,0.625,0.638888888888889,0.652777777777778,
0.666666666666667,0.680555555555556,0.694444444444444,0.708333333333333,
0.722222222222222,0.736111111111111,0.75,0.763888888888889,0.777777777777778,
0.791666666666667,0.805555555555556,0.819444444444444,0.833333333333333,
0.847222222222222,0.861111111111111,0.875,0.888888888888889,0.902777777777778,
0.916666666666667,0.930555555555556,0.944444444444444,0.958333333333333,
0.972222222222222,0.986111111111111,1.),.UNSPECIFIED.)
GEOMETRIC_REPRESENTATION_ITEM()
RATIONAL_B_SPLINE_SURFACE(((1.,0.965925826289068,1.,0.965925826289068,1.,
0.965925826289068,1.,0.965925826289068,1.,0.965925826289068,1.,0.965925826289068,
1.,0.965925826289068,1.,0.965925826289068,1.,0.965925826289068,1.,0.965925826289068,
1.,0.965925826289068,1.,0.965925826289068,1.,0.965925826289068,1.,0.965925826289068,
1.,0.965925826289068,1.,0.965925826289068,1.,0.965925826289068,1.,0.965925826289068,
1.,0.965925826289068,1.,0.965925826289068,1.,0.965925826289068,1.,0.965925826289068,
1.,0.965925826289068,1.,0.965925826289068,1.,0.965925826289068,1.,0.965925826289068,
1.,0.965925826289068,1.,0.965925826289068,1.,0.965925826289068,1.,0.965925826289068,
1.,0.965925826289068,1.,0.965925826289068,1.,0.965925826289068,1.,0.965925826289068,
1.,0.965925826289068,1.,0.965925826289068,1.,0.965925826289068,1.,0.965925826289068,
1.,0.965925826289068,1.,0.965925826289068,1.,0.965925826289068,1.,0.965925826289068,
1.,0.965925826289068,1.,0.965925826289068,1.,0.965925826289068,1.,0.965925826289068,
1.,0.965925826289068,1.,0.965925826289068,1.,0.965925826289068,1.,0.965925826289068,
1.,0.965925826289068,1.,0.965925826289068,1.,0.965925826289068,1.,0.965925826289068,
1.,0.965925826289068,1.,0.965925826289068,1.,0.965925826289068,1.,0.965925826289068,
1.,0.965925826289068,1.,0.965925826289068,1.,0.965925826289068,1.,0.965925826289068,
1.,0.965925826289068,1.,0.965925826289068,1.,0.965925826289068,1.,0.965925826289068,
1.,0.965925826289068,1.,0.965925826289068,1.,0.965925826289068,1.,0.965925826289068,
1.,0.965925826289068,1.,0.965925826289068,1.),(1.,0.965925826289068,1.,
0.965925826289068,1.,0.965925826289068,1.,0.965925826289068,1.,0.965925826289068,
1.,0.965925826289068,1.,0.965925826289068,1.,0.965925826289068,1.,0.965925826289068,
1.,0.965925826289068,1.,0.965925826289068,1.,0.965925826289068,1.,0.965925826289068,
1.,0.965925826289068,1.,0.965925826289068,1.,0.965925826289068,1.,0.965925826289068,
1.,0.965925826289068,1.,0.965925826289068,1.,0.965925826289068,1.,0.965925826289068,
1.,0.965925826289068,1.,0.965925826289068,1.,0.965925826289068,1.,0.965925826289068,
1.,0.965925826289068,1.,0.965925826289068,1.,0.965925826289068,1.,0.965925826289068,
1.,0.965925826289068,1.,0.965925826289068,1.,0.965925826289068,1.,0.965925826289068,
1.,0.965925826289068,1.,0.965925826289068,1.,0.965925826289068,1.,0.965925826289068,
1.,0.965925826289068,1.,0.965925826289068,1.,0.965925826289068,1.,0.965925826289068,
1.,0.965925826289068,1.,0.965925826289068,1.,0.965925826289068,1.,0.965925826289068,
1.,0.965925826289068,1.,0.965925826289068,1.,0.965925826289068,1.,0.965925826289068,
1.,0.965925826289068,1.,0.965925826289068,1.,0.965925826289068,1.,0.965925826289068,
1.,0.965925826289068,1.,0.965925826289068,1.,0.965925826289068,1.,0.965925826289068,
1.,0.965925826289068,1.,0.965925826289068,1.,0.965925826289068,1.,0.965925826289068,
1.,0.965925826289068,1.,0.965925826289068,1.,0.965925826289068,1.,0.965925826289068,
1.,0.965925826289068,1.,0.965925826289068,1.,0.965925826289068,1.,0.965925826289068,
1.,0.965925826289068,1.,0.965925826289068,1.,0.965925826289068,1.)))
REPRESENTATION_ITEM('')
SURFACE()
);
#191=(
BOUNDED_SURFACE()
B_SPLINE_SURFACE(1,2,((#17973,#17974,#17975,#17976,#17977,#17978,#17979,
#17980,#17981,#17982,#17983,#17984,#17985,#17986,#17987,#17988,#17989,#17990,
#17991,#17992,#17993,#17994,#17995,#17996,#17997,#17998,#17999,#18000,#18001,
#18002,#18003,#18004,#18005,#18006,#18007,#18008,#18009,#18010,#18011,#18012,
#18013,#18014,#18015,#18016,#18017,#18018,#18019,#18020,#18021,#18022,#18023,
#18024,#18025,#18026,#18027,#18028,#18029,#18030,#18031,#18032,#18033,#18034,
#18035,#18036,#18037,#18038,#18039,#18040,#18041,#18042,#18043,#18044,#18045,
#18046,#18047,#18048,#18049,#18050,#18051,#18052,#18053,#18054,#18055,#18056,
#18057,#18058,#18059,#18060,#18061,#18062,#18063,#18064,#18065,#18066,#18067,
#18068,#18069,#18070,#18071,#18072,#18073,#18074,#18075,#18076,#18077,#18078,
#18079,#18080,#18081,#18082,#18083,#18084,#18085,#18086,#18087,#18088,#18089,
#18090,#18091,#18092,#18093,#18094,#18095,#18096,#18097,#18098,#18099,#18100,
#18101,#18102,#18103,#18104,#18105,#18106,#18107,#18108,#18109,#18110,#18111,
#18112,#18113,#18114,#18115,#18116,#18117),(#18118,#18119,#18120,#18121,
#18122,#18123,#18124,#18125,#18126,#18127,#18128,#18129,#18130,#18131,#18132,
#18133,#18134,#18135,#18136,#18137,#18138,#18139,#18140,#18141,#18142,#18143,
#18144,#18145,#18146,#18147,#18148,#18149,#18150,#18151,#18152,#18153,#18154,
#18155,#18156,#18157,#18158,#18159,#18160,#18161,#18162,#18163,#18164,#18165,
#18166,#18167,#18168,#18169,#18170,#18171,#18172,#18173,#18174,#18175,#18176,
#18177,#18178,#18179,#18180,#18181,#18182,#18183,#18184,#18185,#18186,#18187,
#18188,#18189,#18190,#18191,#18192,#18193,#18194,#18195,#18196,#18197,#18198,
#18199,#18200,#18201,#18202,#18203,#18204,#18205,#18206,#18207,#18208,#18209,
#18210,#18211,#18212,#18213,#18214,#18215,#18216,#18217,#18218,#18219,#18220,
#18221,#18222,#18223,#18224,#18225,#18226,#18227,#18228,#18229,#18230,#18231,
#18232,#18233,#18234,#18235,#18236,#18237,#18238,#18239,#18240,#18241,#18242,
#18243,#18244,#18245,#18246,#18247,#18248,#18249,#18250,#18251,#18252,#18253,
#18254,#18255,#18256,#18257,#18258,#18259,#18260,#18261,#18262)),
 .UNSPECIFIED.,.F.,.F.,.F.)
B_SPLINE_SURFACE_WITH_KNOTS((2,2),(3,2,2,2,2,2,2,2,2,2,2,2,2,2,2,2,2,2,
2,2,2,2,2,2,2,2,2,2,2,2,2,2,2,2,2,2,2,2,2,2,2,2,2,2,2,2,2,2,2,2,2,2,2,2,
2,2,2,2,2,2,2,2,2,2,2,2,2,2,2,2,2,2,3),(0.,1.),(0.,0.0138888888888889,0.0277777777777778,
0.0416666666666667,0.0555555555555556,0.0694444444444444,0.0833333333333333,
0.0972222222222222,0.111111111111111,0.125,0.138888888888889,0.152777777777778,
0.166666666666667,0.180555555555556,0.194444444444444,0.208333333333333,
0.222222222222222,0.236111111111111,0.25,0.263888888888889,0.277777777777778,
0.291666666666667,0.305555555555556,0.319444444444444,0.333333333333333,
0.347222222222222,0.361111111111111,0.375,0.388888888888889,0.402777777777778,
0.416666666666667,0.430555555555556,0.444444444444444,0.458333333333333,
0.472222222222222,0.486111111111111,0.5,0.513888888888889,0.527777777777778,
0.541666666666667,0.555555555555556,0.569444444444444,0.583333333333333,
0.597222222222222,0.611111111111111,0.625,0.638888888888889,0.652777777777778,
0.666666666666667,0.680555555555556,0.694444444444444,0.708333333333333,
0.722222222222222,0.736111111111111,0.75,0.763888888888889,0.777777777777778,
0.791666666666667,0.805555555555556,0.819444444444444,0.833333333333333,
0.847222222222222,0.861111111111111,0.875,0.888888888888889,0.902777777777778,
0.916666666666667,0.930555555555556,0.944444444444444,0.958333333333333,
0.972222222222222,0.986111111111111,1.),.UNSPECIFIED.)
GEOMETRIC_REPRESENTATION_ITEM()
RATIONAL_B_SPLINE_SURFACE(((1.,0.965925826289068,1.,0.965925826289068,1.,
0.965925826289068,1.,0.965925826289068,1.,0.965925826289068,1.,0.965925826289068,
1.,0.965925826289068,1.,0.965925826289068,1.,0.965925826289068,1.,0.965925826289068,
1.,0.965925826289068,1.,0.965925826289068,1.,0.965925826289068,1.,0.965925826289068,
1.,0.965925826289068,1.,0.965925826289068,1.,0.965925826289068,1.,0.965925826289068,
1.,0.965925826289068,1.,0.965925826289068,1.,0.965925826289068,1.,0.965925826289068,
1.,0.965925826289068,1.,0.965925826289068,1.,0.965925826289068,1.,0.965925826289068,
1.,0.965925826289068,1.,0.965925826289068,1.,0.965925826289068,1.,0.965925826289068,
1.,0.965925826289068,1.,0.965925826289068,1.,0.965925826289068,1.,0.965925826289068,
1.,0.965925826289068,1.,0.965925826289068,1.,0.965925826289068,1.,0.965925826289068,
1.,0.965925826289068,1.,0.965925826289068,1.,0.965925826289068,1.,0.965925826289068,
1.,0.965925826289068,1.,0.965925826289068,1.,0.965925826289068,1.,0.965925826289068,
1.,0.965925826289068,1.,0.965925826289068,1.,0.965925826289068,1.,0.965925826289068,
1.,0.965925826289068,1.,0.965925826289068,1.,0.965925826289068,1.,0.965925826289068,
1.,0.965925826289068,1.,0.965925826289068,1.,0.965925826289068,1.,0.965925826289068,
1.,0.965925826289068,1.,0.965925826289068,1.,0.965925826289068,1.,0.965925826289068,
1.,0.965925826289068,1.,0.965925826289068,1.,0.965925826289068,1.,0.965925826289068,
1.,0.965925826289068,1.,0.965925826289068,1.,0.965925826289068,1.,0.965925826289068,
1.,0.965925826289068,1.,0.965925826289068,1.),(1.,0.965925826289068,1.,
0.965925826289068,1.,0.965925826289068,1.,0.965925826289068,1.,0.965925826289068,
1.,0.965925826289068,1.,0.965925826289068,1.,0.965925826289068,1.,0.965925826289068,
1.,0.965925826289068,1.,0.965925826289068,1.,0.965925826289068,1.,0.965925826289068,
1.,0.965925826289068,1.,0.965925826289068,1.,0.965925826289068,1.,0.965925826289068,
1.,0.965925826289068,1.,0.965925826289068,1.,0.965925826289068,1.,0.965925826289068,
1.,0.965925826289068,1.,0.965925826289068,1.,0.965925826289068,1.,0.965925826289068,
1.,0.965925826289068,1.,0.965925826289068,1.,0.965925826289068,1.,0.965925826289068,
1.,0.965925826289068,1.,0.965925826289068,1.,0.965925826289068,1.,0.965925826289068,
1.,0.965925826289068,1.,0.965925826289068,1.,0.965925826289068,1.,0.965925826289068,
1.,0.965925826289068,1.,0.965925826289068,1.,0.965925826289068,1.,0.965925826289068,
1.,0.965925826289068,1.,0.965925826289068,1.,0.965925826289068,1.,0.965925826289068,
1.,0.965925826289068,1.,0.965925826289068,1.,0.965925826289068,1.,0.965925826289068,
1.,0.965925826289068,1.,0.965925826289068,1.,0.965925826289068,1.,0.965925826289068,
1.,0.965925826289068,1.,0.965925826289068,1.,0.965925826289068,1.,0.965925826289068,
1.,0.965925826289068,1.,0.965925826289068,1.,0.965925826289068,1.,0.965925826289068,
1.,0.965925826289068,1.,0.965925826289068,1.,0.965925826289068,1.,0.965925826289068,
1.,0.965925826289068,1.,0.965925826289068,1.,0.965925826289068,1.,0.965925826289068,
1.,0.965925826289068,1.,0.965925826289068,1.,0.965925826289068,1.)))
REPRESENTATION_ITEM('')
SURFACE()
);
#192=(
BOUNDED_SURFACE()
B_SPLINE_SURFACE(1,2,((#18367,#18368,#18369,#18370,#18371,#18372,#18373,
#18374,#18375,#18376,#18377,#18378,#18379,#18380,#18381,#18382,#18383,#18384,
#18385,#18386,#18387,#18388,#18389,#18390,#18391,#18392,#18393,#18394,#18395,
#18396,#18397,#18398,#18399,#18400,#18401,#18402,#18403,#18404,#18405,#18406,
#18407,#18408,#18409,#18410,#18411,#18412,#18413,#18414,#18415,#18416,#18417,
#18418,#18419,#18420,#18421,#18422,#18423,#18424,#18425,#18426,#18427,#18428,
#18429,#18430,#18431,#18432,#18433,#18434,#18435,#18436,#18437,#18438,#18439,
#18440,#18441,#18442,#18443,#18444,#18445,#18446,#18447,#18448,#18449,#18450,
#18451,#18452,#18453,#18454,#18455,#18456,#18457,#18458,#18459,#18460,#18461,
#18462,#18463,#18464,#18465,#18466,#18467,#18468,#18469,#18470,#18471,#18472,
#18473,#18474,#18475,#18476,#18477,#18478,#18479,#18480,#18481,#18482,#18483,
#18484,#18485,#18486,#18487,#18488,#18489,#18490,#18491,#18492,#18493,#18494,
#18495,#18496,#18497,#18498,#18499,#18500,#18501,#18502,#18503,#18504,#18505,
#18506,#18507,#18508,#18509,#18510,#18511),(#18512,#18513,#18514,#18515,
#18516,#18517,#18518,#18519,#18520,#18521,#18522,#18523,#18524,#18525,#18526,
#18527,#18528,#18529,#18530,#18531,#18532,#18533,#18534,#18535,#18536,#18537,
#18538,#18539,#18540,#18541,#18542,#18543,#18544,#18545,#18546,#18547,#18548,
#18549,#18550,#18551,#18552,#18553,#18554,#18555,#18556,#18557,#18558,#18559,
#18560,#18561,#18562,#18563,#18564,#18565,#18566,#18567,#18568,#18569,#18570,
#18571,#18572,#18573,#18574,#18575,#18576,#18577,#18578,#18579,#18580,#18581,
#18582,#18583,#18584,#18585,#18586,#18587,#18588,#18589,#18590,#18591,#18592,
#18593,#18594,#18595,#18596,#18597,#18598,#18599,#18600,#18601,#18602,#18603,
#18604,#18605,#18606,#18607,#18608,#18609,#18610,#18611,#18612,#18613,#18614,
#18615,#18616,#18617,#18618,#18619,#18620,#18621,#18622,#18623,#18624,#18625,
#18626,#18627,#18628,#18629,#18630,#18631,#18632,#18633,#18634,#18635,#18636,
#18637,#18638,#18639,#18640,#18641,#18642,#18643,#18644,#18645,#18646,#18647,
#18648,#18649,#18650,#18651,#18652,#18653,#18654,#18655,#18656)),
 .UNSPECIFIED.,.F.,.F.,.F.)
B_SPLINE_SURFACE_WITH_KNOTS((2,2),(3,2,2,2,2,2,2,2,2,2,2,2,2,2,2,2,2,2,
2,2,2,2,2,2,2,2,2,2,2,2,2,2,2,2,2,2,2,2,2,2,2,2,2,2,2,2,2,2,2,2,2,2,2,2,
2,2,2,2,2,2,2,2,2,2,2,2,2,2,2,2,2,2,3),(0.,1.00000000985537),(0.,0.0138888888888889,
0.0277777777777778,0.0416666666666667,0.0555555555555556,0.0694444444444444,
0.0833333333333333,0.0972222222222222,0.111111111111111,0.125,0.138888888888889,
0.152777777777778,0.166666666666667,0.180555555555556,0.194444444444444,
0.208333333333333,0.222222222222222,0.236111111111111,0.25,0.263888888888889,
0.277777777777778,0.291666666666667,0.305555555555556,0.319444444444444,
0.333333333333333,0.347222222222222,0.361111111111111,0.375,0.388888888888889,
0.402777777777778,0.416666666666667,0.430555555555556,0.444444444444444,
0.458333333333333,0.472222222222222,0.486111111111111,0.5,0.513888888888889,
0.527777777777778,0.541666666666667,0.555555555555556,0.569444444444444,
0.583333333333333,0.597222222222222,0.611111111111111,0.625,0.638888888888889,
0.652777777777778,0.666666666666667,0.680555555555556,0.694444444444444,
0.708333333333333,0.722222222222222,0.736111111111111,0.75,0.763888888888889,
0.777777777777778,0.791666666666667,0.805555555555556,0.819444444444444,
0.833333333333333,0.847222222222222,0.861111111111111,0.875,0.888888888888889,
0.902777777777778,0.916666666666667,0.930555555555556,0.944444444444444,
0.958333333333333,0.972222222222222,0.986111111111111,1.),.UNSPECIFIED.)
GEOMETRIC_REPRESENTATION_ITEM()
RATIONAL_B_SPLINE_SURFACE(((1.,0.965925826289068,1.,0.965925826289068,1.,
0.965925826289068,1.,0.965925826289068,1.,0.965925826289068,1.,0.965925826289068,
1.,0.965925826289068,1.,0.965925826289068,1.,0.965925826289068,1.,0.965925826289068,
1.,0.965925826289068,1.,0.965925826289068,1.,0.965925826289068,1.,0.965925826289068,
1.,0.965925826289068,1.,0.965925826289068,1.,0.965925826289068,1.,0.965925826289068,
1.,0.965925826289068,1.,0.965925826289068,1.,0.965925826289068,1.,0.965925826289068,
1.,0.965925826289068,1.,0.965925826289068,1.,0.965925826289068,1.,0.965925826289068,
1.,0.965925826289068,1.,0.965925826289068,1.,0.965925826289068,1.,0.965925826289068,
1.,0.965925826289068,1.,0.965925826289068,1.,0.965925826289068,1.,0.965925826289068,
1.,0.965925826289068,1.,0.965925826289068,1.,0.965925826289068,1.,0.965925826289068,
1.,0.965925826289068,1.,0.965925826289068,1.,0.965925826289068,1.,0.965925826289068,
1.,0.965925826289068,1.,0.965925826289068,1.,0.965925826289068,1.,0.965925826289068,
1.,0.965925826289068,1.,0.965925826289068,1.,0.965925826289068,1.,0.965925826289068,
1.,0.965925826289068,1.,0.965925826289068,1.,0.965925826289068,1.,0.965925826289068,
1.,0.965925826289068,1.,0.965925826289068,1.,0.965925826289068,1.,0.965925826289068,
1.,0.965925826289068,1.,0.965925826289068,1.,0.965925826289068,1.,0.965925826289068,
1.,0.965925826289068,1.,0.965925826289068,1.,0.965925826289068,1.,0.965925826289068,
1.,0.965925826289068,1.,0.965925826289068,1.,0.965925826289068,1.,0.965925826289068,
1.,0.965925826289068,1.,0.965925826289068,1.),(1.,0.965925826289068,1.,
0.965925826289068,1.,0.965925826289068,1.,0.965925826289068,1.,0.965925826289068,
1.,0.965925826289068,1.,0.965925826289068,1.,0.965925826289068,1.,0.965925826289068,
1.,0.965925826289068,1.,0.965925826289068,1.,0.965925826289068,1.,0.965925826289068,
1.,0.965925826289068,1.,0.965925826289068,1.,0.965925826289068,1.,0.965925826289068,
1.,0.965925826289068,1.,0.965925826289068,1.,0.965925826289068,1.,0.965925826289068,
1.,0.965925826289068,1.,0.965925826289068,1.,0.965925826289068,1.,0.965925826289068,
1.,0.965925826289068,1.,0.965925826289068,1.,0.965925826289068,1.,0.965925826289068,
1.,0.965925826289068,1.,0.965925826289068,1.,0.965925826289068,1.,0.965925826289068,
1.,0.965925826289068,1.,0.965925826289068,1.,0.965925826289068,1.,0.965925826289068,
1.,0.965925826289068,1.,0.965925826289068,1.,0.965925826289068,1.,0.965925826289068,
1.,0.965925826289068,1.,0.965925826289068,1.,0.965925826289068,1.,0.965925826289068,
1.,0.965925826289068,1.,0.965925826289068,1.,0.965925826289068,1.,0.965925826289068,
1.,0.965925826289068,1.,0.965925826289068,1.,0.965925826289068,1.,0.965925826289068,
1.,0.965925826289068,1.,0.965925826289068,1.,0.965925826289068,1.,0.965925826289068,
1.,0.965925826289068,1.,0.965925826289068,1.,0.965925826289068,1.,0.965925826289068,
1.,0.965925826289068,1.,0.965925826289068,1.,0.965925826289068,1.,0.965925826289068,
1.,0.965925826289068,1.,0.965925826289068,1.,0.965925826289068,1.,0.965925826289068,
1.,0.965925826289068,1.,0.965925826289068,1.,0.965925826289068,1.)))
REPRESENTATION_ITEM('')
SURFACE()
);
#193=(
BOUNDED_SURFACE()
B_SPLINE_SURFACE(1,2,((#18703,#18704,#18705,#18706,#18707,#18708,#18709,
#18710,#18711,#18712,#18713,#18714,#18715,#18716,#18717,#18718,#18719,#18720,
#18721,#18722,#18723,#18724,#18725,#18726,#18727,#18728,#18729,#18730,#18731,
#18732,#18733,#18734,#18735,#18736,#18737,#18738,#18739,#18740,#18741,#18742,
#18743,#18744,#18745,#18746,#18747,#18748,#18749,#18750,#18751,#18752,#18753,
#18754,#18755,#18756,#18757,#18758,#18759,#18760,#18761,#18762,#18763,#18764,
#18765,#18766,#18767,#18768,#18769,#18770,#18771,#18772,#18773,#18774,#18775,
#18776,#18777,#18778,#18779,#18780,#18781,#18782,#18783,#18784,#18785,#18786,
#18787,#18788,#18789,#18790,#18791,#18792,#18793,#18794,#18795,#18796,#18797,
#18798,#18799,#18800,#18801,#18802,#18803,#18804,#18805,#18806,#18807,#18808,
#18809,#18810,#18811,#18812,#18813,#18814,#18815,#18816,#18817,#18818,#18819,
#18820,#18821,#18822,#18823,#18824,#18825,#18826,#18827,#18828,#18829,#18830,
#18831,#18832,#18833,#18834,#18835,#18836,#18837,#18838,#18839,#18840,#18841,
#18842,#18843,#18844,#18845,#18846,#18847),(#18848,#18849,#18850,#18851,
#18852,#18853,#18854,#18855,#18856,#18857,#18858,#18859,#18860,#18861,#18862,
#18863,#18864,#18865,#18866,#18867,#18868,#18869,#18870,#18871,#18872,#18873,
#18874,#18875,#18876,#18877,#18878,#18879,#18880,#18881,#18882,#18883,#18884,
#18885,#18886,#18887,#18888,#18889,#18890,#18891,#18892,#18893,#18894,#18895,
#18896,#18897,#18898,#18899,#18900,#18901,#18902,#18903,#18904,#18905,#18906,
#18907,#18908,#18909,#18910,#18911,#18912,#18913,#18914,#18915,#18916,#18917,
#18918,#18919,#18920,#18921,#18922,#18923,#18924,#18925,#18926,#18927,#18928,
#18929,#18930,#18931,#18932,#18933,#18934,#18935,#18936,#18937,#18938,#18939,
#18940,#18941,#18942,#18943,#18944,#18945,#18946,#18947,#18948,#18949,#18950,
#18951,#18952,#18953,#18954,#18955,#18956,#18957,#18958,#18959,#18960,#18961,
#18962,#18963,#18964,#18965,#18966,#18967,#18968,#18969,#18970,#18971,#18972,
#18973,#18974,#18975,#18976,#18977,#18978,#18979,#18980,#18981,#18982,#18983,
#18984,#18985,#18986,#18987,#18988,#18989,#18990,#18991,#18992)),
 .UNSPECIFIED.,.F.,.F.,.F.)
B_SPLINE_SURFACE_WITH_KNOTS((2,2),(3,2,2,2,2,2,2,2,2,2,2,2,2,2,2,2,2,2,
2,2,2,2,2,2,2,2,2,2,2,2,2,2,2,2,2,2,2,2,2,2,2,2,2,2,2,2,2,2,2,2,2,2,2,2,
2,2,2,2,2,2,2,2,2,2,2,2,2,2,2,2,2,2,3),(0.,1.),(0.,0.0138888888888889,0.0277777777777778,
0.0416666666666667,0.0555555555555556,0.0694444444444444,0.0833333333333333,
0.0972222222222222,0.111111111111111,0.125,0.138888888888889,0.152777777777778,
0.166666666666667,0.180555555555556,0.194444444444444,0.208333333333333,
0.222222222222222,0.236111111111111,0.25,0.263888888888889,0.277777777777778,
0.291666666666667,0.305555555555556,0.319444444444444,0.333333333333333,
0.347222222222222,0.361111111111111,0.375,0.388888888888889,0.402777777777778,
0.416666666666667,0.430555555555556,0.444444444444444,0.458333333333333,
0.472222222222222,0.486111111111111,0.5,0.513888888888889,0.527777777777778,
0.541666666666667,0.555555555555556,0.569444444444444,0.583333333333333,
0.597222222222222,0.611111111111111,0.625,0.638888888888889,0.652777777777778,
0.666666666666667,0.680555555555556,0.694444444444444,0.708333333333333,
0.722222222222222,0.736111111111111,0.75,0.763888888888889,0.777777777777778,
0.791666666666667,0.805555555555556,0.819444444444444,0.833333333333333,
0.847222222222222,0.861111111111111,0.875,0.888888888888889,0.902777777777778,
0.916666666666667,0.930555555555556,0.944444444444444,0.958333333333333,
0.972222222222222,0.986111111111111,1.),.UNSPECIFIED.)
GEOMETRIC_REPRESENTATION_ITEM()
RATIONAL_B_SPLINE_SURFACE(((1.,0.965925826289068,1.,0.965925826289068,1.,
0.965925826289068,1.,0.965925826289068,1.,0.965925826289068,1.,0.965925826289068,
1.,0.965925826289068,1.,0.965925826289068,1.,0.965925826289068,1.,0.965925826289068,
1.,0.965925826289068,1.,0.965925826289068,1.,0.965925826289068,1.,0.965925826289068,
1.,0.965925826289068,1.,0.965925826289068,1.,0.965925826289068,1.,0.965925826289068,
1.,0.965925826289068,1.,0.965925826289068,1.,0.965925826289068,1.,0.965925826289068,
1.,0.965925826289068,1.,0.965925826289068,1.,0.965925826289068,1.,0.965925826289068,
1.,0.965925826289068,1.,0.965925826289068,1.,0.965925826289068,1.,0.965925826289068,
1.,0.965925826289068,1.,0.965925826289068,1.,0.965925826289068,1.,0.965925826289068,
1.,0.965925826289068,1.,0.965925826289068,1.,0.965925826289068,1.,0.965925826289068,
1.,0.965925826289068,1.,0.965925826289068,1.,0.965925826289068,1.,0.965925826289068,
1.,0.965925826289068,1.,0.965925826289068,1.,0.965925826289068,1.,0.965925826289068,
1.,0.965925826289068,1.,0.965925826289068,1.,0.965925826289068,1.,0.965925826289068,
1.,0.965925826289068,1.,0.965925826289068,1.,0.965925826289068,1.,0.965925826289068,
1.,0.965925826289068,1.,0.965925826289068,1.,0.965925826289068,1.,0.965925826289068,
1.,0.965925826289068,1.,0.965925826289068,1.,0.965925826289068,1.,0.965925826289068,
1.,0.965925826289068,1.,0.965925826289068,1.,0.965925826289068,1.,0.965925826289068,
1.,0.965925826289068,1.,0.965925826289068,1.,0.965925826289068,1.,0.965925826289068,
1.,0.965925826289068,1.,0.965925826289068,1.),(1.,0.965925826289068,1.,
0.965925826289068,1.,0.965925826289068,1.,0.965925826289068,1.,0.965925826289068,
1.,0.965925826289068,1.,0.965925826289068,1.,0.965925826289068,1.,0.965925826289068,
1.,0.965925826289068,1.,0.965925826289068,1.,0.965925826289068,1.,0.965925826289068,
1.,0.965925826289068,1.,0.965925826289068,1.,0.965925826289068,1.,0.965925826289068,
1.,0.965925826289068,1.,0.965925826289068,1.,0.965925826289068,1.,0.965925826289068,
1.,0.965925826289068,1.,0.965925826289068,1.,0.965925826289068,1.,0.965925826289068,
1.,0.965925826289068,1.,0.965925826289068,1.,0.965925826289068,1.,0.965925826289068,
1.,0.965925826289068,1.,0.965925826289068,1.,0.965925826289068,1.,0.965925826289068,
1.,0.965925826289068,1.,0.965925826289068,1.,0.965925826289068,1.,0.965925826289068,
1.,0.965925826289068,1.,0.965925826289068,1.,0.965925826289068,1.,0.965925826289068,
1.,0.965925826289068,1.,0.965925826289068,1.,0.965925826289068,1.,0.965925826289068,
1.,0.965925826289068,1.,0.965925826289068,1.,0.965925826289068,1.,0.965925826289068,
1.,0.965925826289068,1.,0.965925826289068,1.,0.965925826289068,1.,0.965925826289068,
1.,0.965925826289068,1.,0.965925826289068,1.,0.965925826289068,1.,0.965925826289068,
1.,0.965925826289068,1.,0.965925826289068,1.,0.965925826289068,1.,0.965925826289068,
1.,0.965925826289068,1.,0.965925826289068,1.,0.965925826289068,1.,0.965925826289068,
1.,0.965925826289068,1.,0.965925826289068,1.,0.965925826289068,1.,0.965925826289068,
1.,0.965925826289068,1.,0.965925826289068,1.,0.965925826289068,1.)))
REPRESENTATION_ITEM('')
SURFACE()
);
#194=(
BOUNDED_SURFACE()
B_SPLINE_SURFACE(1,2,((#19006,#19007,#19008,#19009,#19010,#19011,#19012,
#19013,#19014,#19015,#19016,#19017,#19018,#19019,#19020,#19021,#19022,#19023,
#19024,#19025,#19026,#19027,#19028,#19029,#19030,#19031,#19032,#19033,#19034,
#19035,#19036,#19037,#19038,#19039,#19040,#19041,#19042,#19043,#19044,#19045,
#19046,#19047,#19048,#19049,#19050,#19051,#19052,#19053,#19054,#19055,#19056,
#19057,#19058,#19059,#19060,#19061,#19062,#19063,#19064,#19065,#19066,#19067,
#19068,#19069,#19070,#19071,#19072,#19073,#19074,#19075,#19076,#19077,#19078,
#19079,#19080,#19081,#19082,#19083,#19084,#19085,#19086,#19087,#19088,#19089,
#19090,#19091,#19092,#19093,#19094,#19095,#19096,#19097,#19098,#19099,#19100,
#19101,#19102,#19103,#19104,#19105,#19106,#19107,#19108,#19109,#19110,#19111,
#19112,#19113,#19114,#19115,#19116,#19117,#19118,#19119,#19120,#19121,#19122,
#19123,#19124,#19125,#19126,#19127,#19128,#19129,#19130,#19131,#19132,#19133,
#19134,#19135,#19136,#19137,#19138,#19139,#19140,#19141,#19142,#19143,#19144,
#19145,#19146,#19147,#19148,#19149,#19150),(#19151,#19152,#19153,#19154,
#19155,#19156,#19157,#19158,#19159,#19160,#19161,#19162,#19163,#19164,#19165,
#19166,#19167,#19168,#19169,#19170,#19171,#19172,#19173,#19174,#19175,#19176,
#19177,#19178,#19179,#19180,#19181,#19182,#19183,#19184,#19185,#19186,#19187,
#19188,#19189,#19190,#19191,#19192,#19193,#19194,#19195,#19196,#19197,#19198,
#19199,#19200,#19201,#19202,#19203,#19204,#19205,#19206,#19207,#19208,#19209,
#19210,#19211,#19212,#19213,#19214,#19215,#19216,#19217,#19218,#19219,#19220,
#19221,#19222,#19223,#19224,#19225,#19226,#19227,#19228,#19229,#19230,#19231,
#19232,#19233,#19234,#19235,#19236,#19237,#19238,#19239,#19240,#19241,#19242,
#19243,#19244,#19245,#19246,#19247,#19248,#19249,#19250,#19251,#19252,#19253,
#19254,#19255,#19256,#19257,#19258,#19259,#19260,#19261,#19262,#19263,#19264,
#19265,#19266,#19267,#19268,#19269,#19270,#19271,#19272,#19273,#19274,#19275,
#19276,#19277,#19278,#19279,#19280,#19281,#19282,#19283,#19284,#19285,#19286,
#19287,#19288,#19289,#19290,#19291,#19292,#19293,#19294,#19295)),
 .UNSPECIFIED.,.F.,.F.,.F.)
B_SPLINE_SURFACE_WITH_KNOTS((2,2),(3,2,2,2,2,2,2,2,2,2,2,2,2,2,2,2,2,2,
2,2,2,2,2,2,2,2,2,2,2,2,2,2,2,2,2,2,2,2,2,2,2,2,2,2,2,2,2,2,2,2,2,2,2,2,
2,2,2,2,2,2,2,2,2,2,2,2,2,2,2,2,2,2,3),(0.,1.),(0.,0.0138888888888889,0.0277777777777778,
0.0416666666666667,0.0555555555555556,0.0694444444444444,0.0833333333333333,
0.0972222222222222,0.111111111111111,0.125,0.138888888888889,0.152777777777778,
0.166666666666667,0.180555555555556,0.194444444444444,0.208333333333333,
0.222222222222222,0.236111111111111,0.25,0.263888888888889,0.277777777777778,
0.291666666666667,0.305555555555556,0.319444444444444,0.333333333333333,
0.347222222222222,0.361111111111111,0.375,0.388888888888889,0.402777777777778,
0.416666666666667,0.430555555555556,0.444444444444444,0.458333333333333,
0.472222222222222,0.486111111111111,0.5,0.513888888888889,0.527777777777778,
0.541666666666667,0.555555555555556,0.569444444444444,0.583333333333333,
0.597222222222222,0.611111111111111,0.625,0.638888888888889,0.652777777777778,
0.666666666666667,0.680555555555556,0.694444444444444,0.708333333333333,
0.722222222222222,0.736111111111111,0.75,0.763888888888889,0.777777777777778,
0.791666666666667,0.805555555555556,0.819444444444444,0.833333333333333,
0.847222222222222,0.861111111111111,0.875,0.888888888888889,0.902777777777778,
0.916666666666667,0.930555555555556,0.944444444444444,0.958333333333333,
0.972222222222222,0.986111111111111,1.),.UNSPECIFIED.)
GEOMETRIC_REPRESENTATION_ITEM()
RATIONAL_B_SPLINE_SURFACE(((1.,0.965925826289068,1.,0.965925826289068,1.,
0.965925826289068,1.,0.965925826289068,1.,0.965925826289068,1.,0.965925826289068,
1.,0.965925826289068,1.,0.965925826289068,1.,0.965925826289068,1.,0.965925826289068,
1.,0.965925826289068,1.,0.965925826289068,1.,0.965925826289068,1.,0.965925826289068,
1.,0.965925826289068,1.,0.965925826289068,1.,0.965925826289068,1.,0.965925826289068,
1.,0.965925826289068,1.,0.965925826289068,1.,0.965925826289068,1.,0.965925826289068,
1.,0.965925826289068,1.,0.965925826289068,1.,0.965925826289068,1.,0.965925826289068,
1.,0.965925826289068,1.,0.965925826289068,1.,0.965925826289068,1.,0.965925826289068,
1.,0.965925826289068,1.,0.965925826289068,1.,0.965925826289068,1.,0.965925826289068,
1.,0.965925826289068,1.,0.965925826289068,1.,0.965925826289068,1.,0.965925826289068,
1.,0.965925826289068,1.,0.965925826289068,1.,0.965925826289068,1.,0.965925826289068,
1.,0.965925826289068,1.,0.965925826289068,1.,0.965925826289068,1.,0.965925826289068,
1.,0.965925826289068,1.,0.965925826289068,1.,0.965925826289068,1.,0.965925826289068,
1.,0.965925826289068,1.,0.965925826289068,1.,0.965925826289068,1.,0.965925826289068,
1.,0.965925826289068,1.,0.965925826289068,1.,0.965925826289068,1.,0.965925826289068,
1.,0.965925826289068,1.,0.965925826289068,1.,0.965925826289068,1.,0.965925826289068,
1.,0.965925826289068,1.,0.965925826289068,1.,0.965925826289068,1.,0.965925826289068,
1.,0.965925826289068,1.,0.965925826289068,1.,0.965925826289068,1.,0.965925826289068,
1.,0.965925826289068,1.,0.965925826289068,1.),(1.,0.965925826289068,1.,
0.965925826289068,1.,0.965925826289068,1.,0.965925826289068,1.,0.965925826289068,
1.,0.965925826289068,1.,0.965925826289068,1.,0.965925826289068,1.,0.965925826289068,
1.,0.965925826289068,1.,0.965925826289068,1.,0.965925826289068,1.,0.965925826289068,
1.,0.965925826289068,1.,0.965925826289068,1.,0.965925826289068,1.,0.965925826289068,
1.,0.965925826289068,1.,0.965925826289068,1.,0.965925826289068,1.,0.965925826289068,
1.,0.965925826289068,1.,0.965925826289068,1.,0.965925826289068,1.,0.965925826289068,
1.,0.965925826289068,1.,0.965925826289068,1.,0.965925826289068,1.,0.965925826289068,
1.,0.965925826289068,1.,0.965925826289068,1.,0.965925826289068,1.,0.965925826289068,
1.,0.965925826289068,1.,0.965925826289068,1.,0.965925826289068,1.,0.965925826289068,
1.,0.965925826289068,1.,0.965925826289068,1.,0.965925826289068,1.,0.965925826289068,
1.,0.965925826289068,1.,0.965925826289068,1.,0.965925826289068,1.,0.965925826289068,
1.,0.965925826289068,1.,0.965925826289068,1.,0.965925826289068,1.,0.965925826289068,
1.,0.965925826289068,1.,0.965925826289068,1.,0.965925826289068,1.,0.965925826289068,
1.,0.965925826289068,1.,0.965925826289068,1.,0.965925826289068,1.,0.965925826289068,
1.,0.965925826289068,1.,0.965925826289068,1.,0.965925826289068,1.,0.965925826289068,
1.,0.965925826289068,1.,0.965925826289068,1.,0.965925826289068,1.,0.965925826289068,
1.,0.965925826289068,1.,0.965925826289068,1.,0.965925826289068,1.,0.965925826289068,
1.,0.965925826289068,1.,0.965925826289068,1.,0.965925826289068,1.)))
REPRESENTATION_ITEM('')
SURFACE()
);
#195=(
BOUNDED_SURFACE()
B_SPLINE_SURFACE(1,2,((#19897,#19898,#19899,#19900,#19901,#19902,#19903,
#19904,#19905,#19906,#19907,#19908,#19909,#19910,#19911,#19912,#19913,#19914,
#19915,#19916,#19917,#19918,#19919,#19920,#19921,#19922,#19923,#19924,#19925,
#19926,#19927,#19928,#19929,#19930,#19931,#19932,#19933,#19934,#19935,#19936,
#19937,#19938,#19939,#19940,#19941,#19942,#19943,#19944,#19945,#19946,#19947,
#19948,#19949,#19950,#19951,#19952,#19953,#19954,#19955,#19956,#19957,#19958,
#19959,#19960,#19961,#19962,#19963,#19964,#19965,#19966,#19967,#19968,#19969,
#19970,#19971,#19972,#19973,#19974,#19975,#19976,#19977,#19978,#19979,#19980,
#19981,#19982,#19983,#19984,#19985,#19986,#19987,#19988,#19989),(#19990,
#19991,#19992,#19993,#19994,#19995,#19996,#19997,#19998,#19999,#20000,#20001,
#20002,#20003,#20004,#20005,#20006,#20007,#20008,#20009,#20010,#20011,#20012,
#20013,#20014,#20015,#20016,#20017,#20018,#20019,#20020,#20021,#20022,#20023,
#20024,#20025,#20026,#20027,#20028,#20029,#20030,#20031,#20032,#20033,#20034,
#20035,#20036,#20037,#20038,#20039,#20040,#20041,#20042,#20043,#20044,#20045,
#20046,#20047,#20048,#20049,#20050,#20051,#20052,#20053,#20054,#20055,#20056,
#20057,#20058,#20059,#20060,#20061,#20062,#20063,#20064,#20065,#20066,#20067,
#20068,#20069,#20070,#20071,#20072,#20073,#20074,#20075,#20076,#20077,#20078,
#20079,#20080,#20081,#20082)),.UNSPECIFIED.,.F.,.F.,.F.)
B_SPLINE_SURFACE_WITH_KNOTS((2,2),(3,2,2,2,2,2,2,2,2,2,2,2,2,2,2,2,2,2,
2,2,2,2,2,2,2,2,2,2,2,2,2,2,2,2,2,2,2,2,2,2,2,2,2,2,2,2,3),(0.,1.),(0.,
0.0208333333333333,0.0416666666666667,0.0625,0.0833333333333333,0.104166666666667,
0.125,0.145833333333333,0.166666666666667,0.1875,0.208333333333333,0.229166666666667,
0.25,0.270833333333333,0.291666666666667,0.3125,0.333333333333333,0.354166666666667,
0.375,0.395833333333333,0.416666666666667,0.4375,0.458333333333333,0.479166666666667,
0.5,0.520833333333333,0.541666666666667,0.5625,0.583333333333333,0.604166666666667,
0.625,0.645833333333333,0.666666666666667,0.6875,0.708333333333333,0.729166666666667,
0.75,0.770833333333333,0.791666666666667,0.8125,0.833333333333333,0.854166666666667,
0.875,0.895833333333333,0.916666666666667,0.9375,0.949988556244299),
 .UNSPECIFIED.)
GEOMETRIC_REPRESENTATION_ITEM()
RATIONAL_B_SPLINE_SURFACE(((1.,0.965925826289068,1.,0.965925826289068,1.,
0.965925826289068,1.,0.965925826289068,1.,0.965925826289068,1.,0.965925826289068,
1.,0.965925826289068,1.,0.965925826289068,1.,0.965925826289068,1.,0.965925826289068,
1.,0.965925826289068,1.,0.965925826289068,1.,0.965925826289068,1.,0.965925826289068,
1.,0.965925826289068,1.,0.965925826289068,1.,0.965925826289068,1.,0.965925826289068,
1.,0.965925826289068,1.,0.965925826289068,1.,0.965925826289068,1.,0.965925826289068,
1.,0.965925826289068,1.,0.965925826289068,1.,0.965925826289068,1.,0.965925826289068,
1.,0.965925826289068,1.,0.965925826289068,1.,0.965925826289068,1.,0.965925826289068,
1.,0.965925826289068,1.,0.965925826289068,1.,0.965925826289068,1.,0.965925826289068,
1.,0.965925826289068,1.,0.965925826289068,1.,0.965925826289068,1.,0.965925826289068,
1.,0.965925826289068,1.,0.965925826289068,1.,0.965925826289068,1.,0.965925826289068,
1.,0.965925826289068,1.,0.965925826289068,1.,0.965925826289068,1.,0.979574212726385,
0.98363693040003),(1.,0.965925826289068,1.,0.965925826289068,1.,0.965925826289068,
1.,0.965925826289068,1.,0.965925826289068,1.,0.965925826289068,1.,0.965925826289068,
1.,0.965925826289068,1.,0.965925826289068,1.,0.965925826289068,1.,0.965925826289068,
1.,0.965925826289068,1.,0.965925826289068,1.,0.965925826289068,1.,0.965925826289068,
1.,0.965925826289068,1.,0.965925826289068,1.,0.965925826289068,1.,0.965925826289068,
1.,0.965925826289068,1.,0.965925826289068,1.,0.965925826289068,1.,0.965925826289068,
1.,0.965925826289068,1.,0.965925826289068,1.,0.965925826289068,1.,0.965925826289068,
1.,0.965925826289068,1.,0.965925826289068,1.,0.965925826289068,1.,0.965925826289068,
1.,0.965925826289068,1.,0.965925826289068,1.,0.965925826289068,1.,0.965925826289068,
1.,0.965925826289068,1.,0.965925826289068,1.,0.965925826289068,1.,0.965925826289068,
1.,0.965925826289068,1.,0.965925826289068,1.,0.965925826289068,1.,0.965925826289068,
1.,0.965925826289068,1.,0.965925826289068,1.,0.979574212726385,0.98363693040003)))
REPRESENTATION_ITEM('')
SURFACE()
);
#196=(
BOUNDED_SURFACE()
B_SPLINE_SURFACE(1,2,((#20106,#20107,#20108,#20109,#20110,#20111,#20112,
#20113,#20114,#20115,#20116,#20117,#20118,#20119,#20120,#20121,#20122,#20123,
#20124,#20125,#20126,#20127,#20128,#20129,#20130,#20131,#20132,#20133,#20134,
#20135,#20136,#20137,#20138,#20139,#20140,#20141,#20142,#20143,#20144,#20145,
#20146,#20147,#20148,#20149,#20150,#20151,#20152,#20153,#20154,#20155,#20156,
#20157,#20158,#20159,#20160,#20161,#20162,#20163,#20164,#20165,#20166,#20167,
#20168,#20169,#20170,#20171,#20172,#20173,#20174,#20175,#20176,#20177,#20178,
#20179,#20180,#20181,#20182,#20183,#20184,#20185,#20186,#20187,#20188,#20189,
#20190,#20191,#20192,#20193,#20194,#20195,#20196,#20197,#20198,#20199,#20200),
(#20201,#20202,#20203,#20204,#20205,#20206,#20207,#20208,#20209,#20210,
#20211,#20212,#20213,#20214,#20215,#20216,#20217,#20218,#20219,#20220,#20221,
#20222,#20223,#20224,#20225,#20226,#20227,#20228,#20229,#20230,#20231,#20232,
#20233,#20234,#20235,#20236,#20237,#20238,#20239,#20240,#20241,#20242,#20243,
#20244,#20245,#20246,#20247,#20248,#20249,#20250,#20251,#20252,#20253,#20254,
#20255,#20256,#20257,#20258,#20259,#20260,#20261,#20262,#20263,#20264,#20265,
#20266,#20267,#20268,#20269,#20270,#20271,#20272,#20273,#20274,#20275,#20276,
#20277,#20278,#20279,#20280,#20281,#20282,#20283,#20284,#20285,#20286,#20287,
#20288,#20289,#20290,#20291,#20292,#20293,#20294,#20295)),.UNSPECIFIED.,
 .F.,.F.,.F.)
B_SPLINE_SURFACE_WITH_KNOTS((2,2),(3,2,2,2,2,2,2,2,2,2,2,2,2,2,2,2,2,2,
2,2,2,2,2,2,2,2,2,2,2,2,2,2,2,2,2,2,2,2,2,2,2,2,2,2,2,2,2,3),(0.,1.),(0.,
0.0208333333333333,0.0416666666666667,0.0625,0.0833333333333333,0.104166666666667,
0.125,0.145833333333333,0.166666666666667,0.1875,0.208333333333333,0.229166666666667,
0.25,0.270833333333333,0.291666666666667,0.3125,0.333333333333333,0.354166666666667,
0.375,0.395833333333333,0.416666666666667,0.4375,0.458333333333333,0.479166666666667,
0.5,0.520833333333333,0.541666666666667,0.5625,0.583333333333333,0.604166666666667,
0.625,0.645833333333333,0.666666666666667,0.6875,0.708333333333333,0.729166666666667,
0.75,0.770833333333333,0.791666666666667,0.8125,0.833333333333333,0.854166666666667,
0.875,0.895833333333333,0.916666666666667,0.9375,0.949988555726961,0.95948844128423),
 .UNSPECIFIED.)
GEOMETRIC_REPRESENTATION_ITEM()
RATIONAL_B_SPLINE_SURFACE(((1.,0.965925826289068,1.,0.965925826289068,1.,
0.965925826289068,1.,0.965925826289068,1.,0.965925826289068,1.,0.965925826289068,
1.,0.965925826289068,1.,0.965925826289068,1.,0.965925826289068,1.,0.965925826289068,
1.,0.965925826289068,1.,0.965925826289068,1.,0.965925826289068,1.,0.965925826289068,
1.,0.965925826289068,1.,0.965925826289068,1.,0.965925826289068,1.,0.965925826289068,
1.,0.965925826289068,1.,0.965925826289068,1.,0.965925826289068,1.,0.965925826289068,
1.,0.965925826289068,1.,0.965925826289068,1.,0.965925826289068,1.,0.965925826289068,
1.,0.965925826289068,1.,0.965925826289068,1.,0.965925826289068,1.,0.965925826289068,
1.,0.965925826289068,1.,0.965925826289068,1.,0.965925826289068,1.,0.965925826289068,
1.,0.965925826289068,1.,0.965925826289068,1.,0.965925826289068,1.,0.965925826289068,
1.,0.965925826289068,1.,0.965925826289068,1.,0.965925826289068,1.,0.965925826289068,
1.,0.965925826289068,1.,0.965925826289068,1.,0.965925826289068,1.,0.979574213572523,
0.983636930063434,0.983636930063434,0.983636930063434),(1.,0.965925826289068,
1.,0.965925826289068,1.,0.965925826289068,1.,0.965925826289068,1.,0.965925826289068,
1.,0.965925826289068,1.,0.965925826289068,1.,0.965925826289068,1.,0.965925826289068,
1.,0.965925826289068,1.,0.965925826289068,1.,0.965925826289068,1.,0.965925826289068,
1.,0.965925826289068,1.,0.965925826289068,1.,0.965925826289068,1.,0.965925826289068,
1.,0.965925826289068,1.,0.965925826289068,1.,0.965925826289068,1.,0.965925826289068,
1.,0.965925826289068,1.,0.965925826289068,1.,0.965925826289068,1.,0.965925826289068,
1.,0.965925826289068,1.,0.965925826289068,1.,0.965925826289068,1.,0.965925826289068,
1.,0.965925826289068,1.,0.965925826289068,1.,0.965925826289068,1.,0.965925826289068,
1.,0.965925826289068,1.,0.965925826289068,1.,0.965925826289068,1.,0.965925826289068,
1.,0.965925826289068,1.,0.965925826289068,1.,0.965925826289068,1.,0.965925826289068,
1.,0.965925826289068,1.,0.965925826289068,1.,0.965925826289068,1.,0.965925826289068,
1.,0.979574213572523,0.983636930063434,0.983636930063434,0.983636930063434)))
REPRESENTATION_ITEM('')
SURFACE()
);
#197=(
BOUNDED_CURVE()
B_SPLINE_CURVE(2,(#5212,#5213,#5214,#5215,#5216,#5217,#5218),
 .UNSPECIFIED.,.F.,.F.)
B_SPLINE_CURVE_WITH_KNOTS((3,2,2,3),(0.710433099667006,0.722222222222222,
0.736111111111111,0.747484081398396),.UNSPECIFIED.)
CURVE()
GEOMETRIC_REPRESENTATION_ITEM()
RATIONAL_B_SPLINE_CURVE((0.991254739061418,0.971077268091095,1.,0.965925826289068,
1.,0.97209823130717,0.989891404642439))
REPRESENTATION_ITEM('')
);
#198=(
BOUNDED_CURVE()
B_SPLINE_CURVE(2,(#5221,#5222,#5223,#5224,#5225,#5226,#5227),
 .UNSPECIFIED.,.F.,.F.)
B_SPLINE_CURVE_WITH_KNOTS((3,2,2,3),(0.543766433000339,0.555555555555556,
0.569444444444444,0.580817414731729),.UNSPECIFIED.)
CURVE()
GEOMETRIC_REPRESENTATION_ITEM()
RATIONAL_B_SPLINE_CURVE((0.991254739061418,0.971077268091095,1.,0.965925826289068,
1.,0.97209823130717,0.989891404642439))
REPRESENTATION_ITEM('')
);
#199=(
BOUNDED_CURVE()
B_SPLINE_CURVE(2,(#5233,#5234,#5235,#5236,#5237,#5238,#5239),
 .UNSPECIFIED.,.F.,.F.)
B_SPLINE_CURVE_WITH_KNOTS((3,2,2,3),(0.585429670084067,0.597222222222222,
0.611111111111111,0.622900233666328),.UNSPECIFIED.)
CURVE()
GEOMETRIC_REPRESENTATION_ITEM()
RATIONAL_B_SPLINE_CURVE((0.991266482904706,0.971068854156347,1.,0.965925826289068,
1.,0.971077268091093,0.99125473906142))
REPRESENTATION_ITEM('')
);
#200=(
BOUNDED_CURVE()
B_SPLINE_CURVE(2,(#5245,#5246,#5247,#5248,#5249,#5250,#5251),
 .UNSPECIFIED.,.F.,.F.)
B_SPLINE_CURVE_WITH_KNOTS((3,2,2,3),(0.752096336750733,0.763888888888889,
0.777777777777778,0.78959636025962),.UNSPECIFIED.)
CURVE()
GEOMETRIC_REPRESENTATION_ITEM()
RATIONAL_B_SPLINE_CURVE((0.991266482904706,0.971068854156347,1.,0.965925826289068,
1.,0.971004992859764,0.991355888936111))
REPRESENTATION_ITEM('')
);
#201=(
BOUNDED_CURVE()
B_SPLINE_CURVE(2,(#5257,#5258,#5259,#5260,#5261,#5262,#5263),
 .UNSPECIFIED.,.F.,.F.)
B_SPLINE_CURVE_WITH_KNOTS((3,2,2,3),(0.210433099667006,0.222222222222222,
0.236111111111111,0.247484081398396),.UNSPECIFIED.)
CURVE()
GEOMETRIC_REPRESENTATION_ITEM()
RATIONAL_B_SPLINE_CURVE((0.991254739061418,0.971077268091095,1.,0.965925826289068,
1.,0.97209823130717,0.989891404642439))
REPRESENTATION_ITEM('')
);
#202=(
BOUNDED_CURVE()
B_SPLINE_CURVE(2,(#5266,#5267,#5268,#5269,#5270,#5271,#5272),
 .UNSPECIFIED.,.F.,.F.)
B_SPLINE_CURVE_WITH_KNOTS((3,2,2,3),(0.0437664330003391,0.0555555555555556,
0.0694444444444444,0.080817414731729),.UNSPECIFIED.)
CURVE()
GEOMETRIC_REPRESENTATION_ITEM()
RATIONAL_B_SPLINE_CURVE((0.991254739061418,0.971077268091094,1.,0.965925826289068,
1.,0.97209823130717,0.989891404642439))
REPRESENTATION_ITEM('')
);
#203=(
BOUNDED_CURVE()
B_SPLINE_CURVE(2,(#5278,#5279,#5280,#5281,#5282,#5283,#5284),
 .UNSPECIFIED.,.F.,.F.)
B_SPLINE_CURVE_WITH_KNOTS((3,2,2,3),(0.0854296700840668,0.0972222222222222,
0.111111111111111,0.122900233666328),.UNSPECIFIED.)
CURVE()
GEOMETRIC_REPRESENTATION_ITEM()
RATIONAL_B_SPLINE_CURVE((0.991266482904706,0.971068854156348,1.,0.965925826289068,
1.,0.971077268091095,0.991254739061418))
REPRESENTATION_ITEM('')
);
#204=(
BOUNDED_CURVE()
B_SPLINE_CURVE(2,(#5287,#5288,#5289,#5290,#5291,#5292,#5293),
 .UNSPECIFIED.,.F.,.F.)
B_SPLINE_CURVE_WITH_KNOTS((3,2,2,3),(0.252096336750733,0.263888888888889,
0.277777777777778,0.289566900332994),.UNSPECIFIED.)
CURVE()
GEOMETRIC_REPRESENTATION_ITEM()
RATIONAL_B_SPLINE_CURVE((0.991266482904706,0.971068854156347,1.,0.965925826289068,
1.,0.971077268091095,0.991254739061418))
REPRESENTATION_ITEM('')
);
#205=(
BOUNDED_CURVE()
B_SPLINE_CURVE(2,(#5299,#5300,#5301,#5302,#5303,#5304,#5305),
 .UNSPECIFIED.,.F.,.F.)
B_SPLINE_CURVE_WITH_KNOTS((3,2,2,3),(0.377099766333672,0.388888888888889,
0.402777777777778,0.414150748065062),.UNSPECIFIED.)
CURVE()
GEOMETRIC_REPRESENTATION_ITEM()
RATIONAL_B_SPLINE_CURVE((0.991254739061418,0.971077268091095,1.,0.965925826289068,
1.,0.97209823130717,0.989891404642439))
REPRESENTATION_ITEM('')
);
#206=(
BOUNDED_CURVE()
B_SPLINE_CURVE(2,(#5308,#5309,#5310,#5311,#5312,#5313,#5314),
 .UNSPECIFIED.,.F.,.F.)
B_SPLINE_CURVE_WITH_KNOTS((3,2,2,3),(0.210433099667006,0.222222222222222,
0.236111111111111,0.247484081398396),.UNSPECIFIED.)
CURVE()
GEOMETRIC_REPRESENTATION_ITEM()
RATIONAL_B_SPLINE_CURVE((0.991254739061418,0.971077268091095,1.,0.965925826289068,
1.,0.97209823130717,0.989891404642439))
REPRESENTATION_ITEM('')
);
#207=(
BOUNDED_CURVE()
B_SPLINE_CURVE(2,(#5320,#5321,#5322,#5323,#5324,#5325,#5326),
 .UNSPECIFIED.,.F.,.F.)
B_SPLINE_CURVE_WITH_KNOTS((3,2,2,3),(0.252096336750733,0.263888888888889,
0.277777777777778,0.289566900332994),.UNSPECIFIED.)
CURVE()
GEOMETRIC_REPRESENTATION_ITEM()
RATIONAL_B_SPLINE_CURVE((0.991266482904706,0.971068854156347,1.,0.965925826289068,
1.,0.971077268091095,0.991254739061418))
REPRESENTATION_ITEM('')
);
#208=(
BOUNDED_CURVE()
B_SPLINE_CURVE(2,(#5329,#5330,#5331,#5332,#5333,#5334,#5335),
 .UNSPECIFIED.,.F.,.F.)
B_SPLINE_CURVE_WITH_KNOTS((3,2,2,3),(0.4187630034174,0.430555555555556,
0.444444444444444,0.456233566999661),.UNSPECIFIED.)
CURVE()
GEOMETRIC_REPRESENTATION_ITEM()
RATIONAL_B_SPLINE_CURVE((0.991266482904706,0.971068854156347,1.,0.965925826289068,
1.,0.971077268091095,0.991254739061418))
REPRESENTATION_ITEM('')
);
#209=(
BOUNDED_CURVE()
B_SPLINE_CURVE(2,(#5341,#5342,#5343,#5344,#5345,#5346,#5347),
 .UNSPECIFIED.,.F.,.F.)
B_SPLINE_CURVE_WITH_KNOTS((3,2,2,3),(0.543766433000339,0.555555555555556,
0.569444444444444,0.580817414731729),.UNSPECIFIED.)
CURVE()
GEOMETRIC_REPRESENTATION_ITEM()
RATIONAL_B_SPLINE_CURVE((0.991254739061418,0.971077268091094,1.,0.965925826289068,
1.,0.97209823130717,0.989891404642439))
REPRESENTATION_ITEM('')
);
#210=(
BOUNDED_CURVE()
B_SPLINE_CURVE(2,(#5350,#5351,#5352,#5353,#5354,#5355,#5356),
 .UNSPECIFIED.,.F.,.F.)
B_SPLINE_CURVE_WITH_KNOTS((3,2,2,3),(0.377099766333672,0.388888888888889,
0.402777777777778,0.414150748065062),.UNSPECIFIED.)
CURVE()
GEOMETRIC_REPRESENTATION_ITEM()
RATIONAL_B_SPLINE_CURVE((0.991254739061418,0.971077268091095,1.,0.965925826289068,
1.,0.97209823130717,0.989891404642439))
REPRESENTATION_ITEM('')
);
#211=(
BOUNDED_CURVE()
B_SPLINE_CURVE(2,(#5362,#5363,#5364,#5365,#5366,#5367,#5368),
 .UNSPECIFIED.,.F.,.F.)
B_SPLINE_CURVE_WITH_KNOTS((3,2,2,3),(0.4187630034174,0.430555555555556,
0.444444444444444,0.456233566999661),.UNSPECIFIED.)
CURVE()
GEOMETRIC_REPRESENTATION_ITEM()
RATIONAL_B_SPLINE_CURVE((0.991266482904706,0.971068854156347,1.,0.965925826289068,
1.,0.971077268091095,0.991254739061418))
REPRESENTATION_ITEM('')
);
#212=(
BOUNDED_CURVE()
B_SPLINE_CURVE(2,(#5371,#5372,#5373,#5374,#5375,#5376,#5377),
 .UNSPECIFIED.,.F.,.F.)
B_SPLINE_CURVE_WITH_KNOTS((3,2,2,3),(0.585429670084067,0.597222222222222,
0.611111111111111,0.622900233666328),.UNSPECIFIED.)
CURVE()
GEOMETRIC_REPRESENTATION_ITEM()
RATIONAL_B_SPLINE_CURVE((0.991266482904706,0.971068854156347,1.,0.965925826289068,
1.,0.971077268091095,0.991254739061418))
REPRESENTATION_ITEM('')
);
#213=(
BOUNDED_CURVE()
B_SPLINE_CURVE(2,(#5383,#5384,#5385,#5386,#5387,#5388,#5389),
 .UNSPECIFIED.,.F.,.F.)
B_SPLINE_CURVE_WITH_KNOTS((3,2,2,3),(0.00251591860160435,0.0138888888888889,
0.0277777777777778,0.039154184928472),.UNSPECIFIED.)
CURVE()
GEOMETRIC_REPRESENTATION_ITEM()
RATIONAL_B_SPLINE_CURVE((0.989891404642439,0.97209823130717,1.,0.965925826289068,
1.,0.972089799510949,0.989902162858515))
REPRESENTATION_ITEM('')
);
#214=(
BOUNDED_CURVE()
B_SPLINE_CURVE(2,(#5392,#5393,#5394,#5395,#5396,#5397,#5398),
 .UNSPECIFIED.,.F.,.F.)
B_SPLINE_CURVE_WITH_KNOTS((3,2,2,3),(0.169182585268271,0.180555555555556,
0.194444444444444,0.205820851595139),.UNSPECIFIED.)
CURVE()
GEOMETRIC_REPRESENTATION_ITEM()
RATIONAL_B_SPLINE_CURVE((0.989891404642439,0.97209823130717,1.,0.965925826289068,
1.,0.972089799510949,0.989902162858515))
REPRESENTATION_ITEM('')
);
#215=(
BOUNDED_CURVE()
B_SPLINE_CURVE(2,(#5404,#5405,#5406,#5407,#5408,#5409,#5410),
 .UNSPECIFIED.,.F.,.F.)
B_SPLINE_CURVE_WITH_KNOTS((3,2,2,3),(0.127512481738195,0.138888888888889,
0.152777777777778,0.164570329915933),.UNSPECIFIED.)
CURVE()
GEOMETRIC_REPRESENTATION_ITEM()
RATIONAL_B_SPLINE_CURVE((0.989902162858515,0.972089799510949,1.,0.965925826289068,
1.,0.971068854156348,0.991266482904706))
REPRESENTATION_ITEM('')
);
#216=(
BOUNDED_CURVE()
B_SPLINE_CURVE(2,(#5419,#5420,#5421,#5422,#5423,#5424,#5425),
 .UNSPECIFIED.,.F.,.F.)
B_SPLINE_CURVE_WITH_KNOTS((3,2,2,3),(0.169182585268271,0.180555555555556,
0.194444444444444,0.205820851595139),.UNSPECIFIED.)
CURVE()
GEOMETRIC_REPRESENTATION_ITEM()
RATIONAL_B_SPLINE_CURVE((0.989891404642439,0.97209823130717,1.,0.965925826289068,
1.,0.972089799510949,0.989902162858515))
REPRESENTATION_ITEM('')
);
#217=(
BOUNDED_CURVE()
B_SPLINE_CURVE(2,(#5428,#5429,#5430,#5431,#5432,#5433,#5434),
 .UNSPECIFIED.,.F.,.F.)
B_SPLINE_CURVE_WITH_KNOTS((3,2,2,3),(0.335849251934938,0.347222222222222,
0.361111111111111,0.372487518261805),.UNSPECIFIED.)
CURVE()
GEOMETRIC_REPRESENTATION_ITEM()
RATIONAL_B_SPLINE_CURVE((0.989891404642439,0.97209823130717,1.,0.965925826289068,
1.,0.972089799510949,0.989902162858515))
REPRESENTATION_ITEM('')
);
#218=(
BOUNDED_CURVE()
B_SPLINE_CURVE(2,(#5440,#5441,#5442,#5443,#5444,#5445,#5446),
 .UNSPECIFIED.,.F.,.F.)
B_SPLINE_CURVE_WITH_KNOTS((3,2,2,3),(0.294179148404861,0.305555555555556,
0.319444444444444,0.3312369965826),.UNSPECIFIED.)
CURVE()
GEOMETRIC_REPRESENTATION_ITEM()
RATIONAL_B_SPLINE_CURVE((0.989902162858515,0.972089799510949,1.,0.965925826289068,
1.,0.971068854156348,0.991266482904706))
REPRESENTATION_ITEM('')
);
#219=(
BOUNDED_CURVE()
B_SPLINE_CURVE(2,(#5449,#5450,#5451,#5452,#5453,#5454,#5455),
 .UNSPECIFIED.,.F.,.F.)
B_SPLINE_CURVE_WITH_KNOTS((3,2,2,3),(0.127512481738195,0.138888888888889,
0.152777777777778,0.164570329915933),.UNSPECIFIED.)
CURVE()
GEOMETRIC_REPRESENTATION_ITEM()
RATIONAL_B_SPLINE_CURVE((0.989902162858515,0.972089799510949,1.,0.965925826289068,
1.,0.971068854156348,0.991266482904706))
REPRESENTATION_ITEM('')
);
#220=(
BOUNDED_CURVE()
B_SPLINE_CURVE(2,(#5461,#5462,#5463,#5464,#5465,#5466,#5467),
 .UNSPECIFIED.,.F.,.F.)
B_SPLINE_CURVE_WITH_KNOTS((3,2,2,3),(0.335849251934938,0.347222222222222,
0.361111111111111,0.372487518261805),.UNSPECIFIED.)
CURVE()
GEOMETRIC_REPRESENTATION_ITEM()
RATIONAL_B_SPLINE_CURVE((0.989891404642439,0.97209823130717,1.,0.965925826289068,
1.,0.972089799510949,0.989902162858515))
REPRESENTATION_ITEM('')
);
#221=(
BOUNDED_CURVE()
B_SPLINE_CURVE(2,(#5470,#5471,#5472,#5473,#5474,#5475,#5476),
 .UNSPECIFIED.,.F.,.F.)
B_SPLINE_CURVE_WITH_KNOTS((3,2,2,3),(0.502515918601604,0.513888888888889,
0.527777777777778,0.539154184928472),.UNSPECIFIED.)
CURVE()
GEOMETRIC_REPRESENTATION_ITEM()
RATIONAL_B_SPLINE_CURVE((0.989891404642439,0.97209823130717,1.,0.965925826289068,
1.,0.972089799510949,0.989902162858515))
REPRESENTATION_ITEM('')
);
#222=(
BOUNDED_CURVE()
B_SPLINE_CURVE(2,(#5482,#5483,#5484,#5485,#5486,#5487,#5488),
 .UNSPECIFIED.,.F.,.F.)
B_SPLINE_CURVE_WITH_KNOTS((3,2,2,3),(0.460845815071528,0.472222222222222,
0.486111111111111,0.497903663249267),.UNSPECIFIED.)
CURVE()
GEOMETRIC_REPRESENTATION_ITEM()
RATIONAL_B_SPLINE_CURVE((0.989902162858515,0.972089799510949,1.,0.965925826289068,
1.,0.971068854156348,0.991266482904706))
REPRESENTATION_ITEM('')
);
#223=(
BOUNDED_CURVE()
B_SPLINE_CURVE(2,(#5491,#5492,#5493,#5494,#5495,#5496,#5497),
 .UNSPECIFIED.,.F.,.F.)
B_SPLINE_CURVE_WITH_KNOTS((3,2,2,3),(0.294179148404861,0.305555555555556,
0.319444444444444,0.3312369965826),.UNSPECIFIED.)
CURVE()
GEOMETRIC_REPRESENTATION_ITEM()
RATIONAL_B_SPLINE_CURVE((0.989902162858515,0.972089799510949,1.,0.965925826289068,
1.,0.971068854156348,0.991266482904706))
REPRESENTATION_ITEM('')
);
#224=(
BOUNDED_CURVE()
B_SPLINE_CURVE(2,(#5503,#5504,#5505,#5506,#5507,#5508,#5509),
 .UNSPECIFIED.,.F.,.F.)
B_SPLINE_CURVE_WITH_KNOTS((3,2,2,3),(0.502515918601604,0.513888888888889,
0.527777777777778,0.539154184928472),.UNSPECIFIED.)
CURVE()
GEOMETRIC_REPRESENTATION_ITEM()
RATIONAL_B_SPLINE_CURVE((0.989891404642439,0.97209823130717,1.,0.965925826289068,
1.,0.972089799510949,0.989902162858515))
REPRESENTATION_ITEM('')
);
#225=(
BOUNDED_CURVE()
B_SPLINE_CURVE(2,(#5512,#5513,#5514,#5515,#5516,#5517,#5518),
 .UNSPECIFIED.,.F.,.F.)
B_SPLINE_CURVE_WITH_KNOTS((3,2,2,3),(0.669182585268271,0.680555555555556,
0.694444444444444,0.705820851595139),.UNSPECIFIED.)
CURVE()
GEOMETRIC_REPRESENTATION_ITEM()
RATIONAL_B_SPLINE_CURVE((0.989891404642439,0.97209823130717,1.,0.965925826289068,
1.,0.972089799510949,0.989902162858515))
REPRESENTATION_ITEM('')
);
#226=(
BOUNDED_CURVE()
B_SPLINE_CURVE(2,(#5524,#5525,#5526,#5527,#5528,#5529,#5530),
 .UNSPECIFIED.,.F.,.F.)
B_SPLINE_CURVE_WITH_KNOTS((3,2,2,3),(0.627512481738195,0.638888888888889,
0.652777777777778,0.664570329915933),.UNSPECIFIED.)
CURVE()
GEOMETRIC_REPRESENTATION_ITEM()
RATIONAL_B_SPLINE_CURVE((0.989902162858515,0.972089799510949,1.,0.965925826289068,
1.,0.971068854156347,0.991266482904706))
REPRESENTATION_ITEM('')
);
#227=(
BOUNDED_CURVE()
B_SPLINE_CURVE(2,(#5533,#5534,#5535,#5536,#5537,#5538,#5539),
 .UNSPECIFIED.,.F.,.F.)
B_SPLINE_CURVE_WITH_KNOTS((3,2,2,3),(0.460845815071528,0.472222222222222,
0.486111111111111,0.497903663249267),.UNSPECIFIED.)
CURVE()
GEOMETRIC_REPRESENTATION_ITEM()
RATIONAL_B_SPLINE_CURVE((0.989902162858515,0.972089799510949,1.,0.965925826289068,
1.,0.971068854156348,0.991266482904706))
REPRESENTATION_ITEM('')
);
#228=(
BOUNDED_CURVE()
B_SPLINE_CURVE(2,(#5832,#5833,#5834,#5835,#5836,#5837,#5838),
 .UNSPECIFIED.,.F.,.F.)
B_SPLINE_CURVE_WITH_KNOTS((3,2,2,3),(0.0436499985776507,0.0555555555555556,
0.0694444444444444,0.0809569637747658),.UNSPECIFIED.)
CURVE()
GEOMETRIC_REPRESENTATION_ITEM()
RATIONAL_B_SPLINE_CURVE((0.991658091170858,0.970791614805482,1.,0.965925826289068,
1.,0.971755869987148,0.99033493732901))
REPRESENTATION_ITEM('')
);
#229=(
BOUNDED_CURVE()
B_SPLINE_CURVE(2,(#6146,#6147,#6148,#6149,#6150,#6151,#6152),
 .UNSPECIFIED.,.F.,.F.)
B_SPLINE_CURVE_WITH_KNOTS((3,2,2,3),(0.0853134259903282,0.0972222222222222,
0.111111111111111,0.123016668089016),.UNSPECIFIED.)
CURVE()
GEOMETRIC_REPRESENTATION_ITEM()
RATIONAL_B_SPLINE_CURVE((0.991669449544642,0.970783667812458,1.,0.965925826289068,
1.,0.970791614805482,0.991658091170858))
REPRESENTATION_ITEM('')
);
#230=(
BOUNDED_CURVE()
B_SPLINE_CURVE(2,(#6454,#6455,#6456,#6457,#6458,#6459,#6460),
 .UNSPECIFIED.,.F.,.F.)
B_SPLINE_CURVE_WITH_KNOTS((3,2,2,3),(0.210316665244317,0.222222222222222,
0.236111111111111,0.247623630441432),.UNSPECIFIED.)
CURVE()
GEOMETRIC_REPRESENTATION_ITEM()
RATIONAL_B_SPLINE_CURVE((0.991658091170858,0.970791614805482,1.,0.965925826289068,
1.,0.971755869987148,0.99033493732901))
REPRESENTATION_ITEM('')
);
#231=(
BOUNDED_CURVE()
B_SPLINE_CURVE(2,(#6768,#6769,#6770,#6771,#6772,#6773,#6774),
 .UNSPECIFIED.,.F.,.F.)
B_SPLINE_CURVE_WITH_KNOTS((3,2,2,3),(0.251980092656995,0.263888888888889,
0.277777777777778,0.289683334755683),.UNSPECIFIED.)
CURVE()
GEOMETRIC_REPRESENTATION_ITEM()
RATIONAL_B_SPLINE_CURVE((0.991669449544642,0.970783667812457,1.,0.965925826289068,
1.,0.970791614805482,0.991658091170858))
REPRESENTATION_ITEM('')
);
#232=(
BOUNDED_CURVE()
B_SPLINE_CURVE(2,(#7076,#7077,#7078,#7079,#7080,#7081,#7082),
 .UNSPECIFIED.,.F.,.F.)
B_SPLINE_CURVE_WITH_KNOTS((3,2,2,3),(0.376983331910984,0.388888888888889,
0.402777777777778,0.414290297108099),.UNSPECIFIED.)
CURVE()
GEOMETRIC_REPRESENTATION_ITEM()
RATIONAL_B_SPLINE_CURVE((0.991658091170857,0.970791614805482,1.,0.965925826289068,
1.,0.971755869987148,0.99033493732901))
REPRESENTATION_ITEM('')
);
#233=(
BOUNDED_CURVE()
B_SPLINE_CURVE(2,(#7390,#7391,#7392,#7393,#7394,#7395,#7396),
 .UNSPECIFIED.,.F.,.F.)
B_SPLINE_CURVE_WITH_KNOTS((3,2,2,3),(0.418646759323662,0.430555555555556,
0.444444444444444,0.456350001422349),.UNSPECIFIED.)
CURVE()
GEOMETRIC_REPRESENTATION_ITEM()
RATIONAL_B_SPLINE_CURVE((0.991669449544642,0.970783667812457,1.,0.965925826289068,
1.,0.970791614805482,0.991658091170858))
REPRESENTATION_ITEM('')
);
#234=(
BOUNDED_CURVE()
B_SPLINE_CURVE(2,(#7698,#7699,#7700,#7701,#7702,#7703,#7704),
 .UNSPECIFIED.,.F.,.F.)
B_SPLINE_CURVE_WITH_KNOTS((3,2,2,3),(0.543649998577651,0.555555555555556,
0.569444444444444,0.580956963774766),.UNSPECIFIED.)
CURVE()
GEOMETRIC_REPRESENTATION_ITEM()
RATIONAL_B_SPLINE_CURVE((0.991658091170858,0.970791614805482,1.,0.965925826289068,
1.,0.971755869987148,0.99033493732901))
REPRESENTATION_ITEM('')
);
#235=(
BOUNDED_CURVE()
B_SPLINE_CURVE(2,(#8012,#8013,#8014,#8015,#8016,#8017,#8018),
 .UNSPECIFIED.,.F.,.F.)
B_SPLINE_CURVE_WITH_KNOTS((3,2,2,3),(0.585313425990328,0.597222222222222,
0.611111111111111,0.623016668089016),.UNSPECIFIED.)
CURVE()
GEOMETRIC_REPRESENTATION_ITEM()
RATIONAL_B_SPLINE_CURVE((0.991669449544642,0.970783667812458,1.,0.965925826289068,
1.,0.970791614805482,0.991658091170858))
REPRESENTATION_ITEM('')
);
#236=(
BOUNDED_CURVE()
B_SPLINE_CURVE(2,(#8336,#8337,#8338,#8339,#8340,#8341,#8342),
 .UNSPECIFIED.,.F.,.F.)
B_SPLINE_CURVE_WITH_KNOTS((3,2,2,3),(0.00237636955856754,0.0138888888888889,
0.0277777777777778,0.0392935428934596),.UNSPECIFIED.)
CURVE()
GEOMETRIC_REPRESENTATION_ITEM()
RATIONAL_B_SPLINE_CURVE((0.99033493732901,0.971755869987148,1.,0.965925826289068,
1.,0.971747906970446,0.990345417239974))
REPRESENTATION_ITEM('')
);
#237=(
BOUNDED_CURVE()
B_SPLINE_CURVE(2,(#8643,#8644,#8645,#8646,#8647,#8648,#8649),
 .UNSPECIFIED.,.F.,.F.)
B_SPLINE_CURVE_WITH_KNOTS((3,2,2,3),(0.169043036225234,0.180555555555556,
0.194444444444444,0.205960209560126),.UNSPECIFIED.)
CURVE()
GEOMETRIC_REPRESENTATION_ITEM()
RATIONAL_B_SPLINE_CURVE((0.99033493732901,0.971755869987148,1.,0.965925826289068,
1.,0.971747906970446,0.990345417239974))
REPRESENTATION_ITEM('')
);
#238=(
BOUNDED_CURVE()
B_SPLINE_CURVE(2,(#8943,#8944,#8945,#8946,#8947,#8948,#8949),
 .UNSPECIFIED.,.F.,.F.)
B_SPLINE_CURVE_WITH_KNOTS((3,2,2,3),(0.127373123773207,0.138888888888889,
0.152777777777778,0.164686574009672),.UNSPECIFIED.)
CURVE()
GEOMETRIC_REPRESENTATION_ITEM()
RATIONAL_B_SPLINE_CURVE((0.990345417239974,0.971747906970446,1.,0.965925826289068,
1.,0.970783667812458,0.991669449544642))
REPRESENTATION_ITEM('')
);
#239=(
BOUNDED_CURVE()
B_SPLINE_CURVE(2,(#9265,#9266,#9267,#9268,#9269,#9270,#9271),
 .UNSPECIFIED.,.F.,.F.)
B_SPLINE_CURVE_WITH_KNOTS((3,2,2,3),(0.335709702891901,0.347222222222222,
0.361111111111111,0.372626876226793),.UNSPECIFIED.)
CURVE()
GEOMETRIC_REPRESENTATION_ITEM()
RATIONAL_B_SPLINE_CURVE((0.99033493732901,0.971755869987148,1.,0.965925826289068,
1.,0.971747906970446,0.990345417239974))
REPRESENTATION_ITEM('')
);
#240=(
BOUNDED_CURVE()
B_SPLINE_CURVE(2,(#9565,#9566,#9567,#9568,#9569,#9570,#9571),
 .UNSPECIFIED.,.F.,.F.)
B_SPLINE_CURVE_WITH_KNOTS((3,2,2,3),(0.294039790439874,0.305555555555556,
0.319444444444444,0.331353240676338),.UNSPECIFIED.)
CURVE()
GEOMETRIC_REPRESENTATION_ITEM()
RATIONAL_B_SPLINE_CURVE((0.990345417239974,0.971747906970446,1.,0.965925826289068,
1.,0.970783667812457,0.991669449544642))
REPRESENTATION_ITEM('')
);
#241=(
BOUNDED_CURVE()
B_SPLINE_CURVE(2,(#9887,#9888,#9889,#9890,#9891,#9892,#9893),
 .UNSPECIFIED.,.F.,.F.)
B_SPLINE_CURVE_WITH_KNOTS((3,2,2,3),(0.502376369558567,0.513888888888889,
0.527777777777778,0.53929354289346),.UNSPECIFIED.)
CURVE()
GEOMETRIC_REPRESENTATION_ITEM()
RATIONAL_B_SPLINE_CURVE((0.99033493732901,0.971755869987148,1.,0.965925826289068,
1.,0.971747906970446,0.990345417239974))
REPRESENTATION_ITEM('')
);
#242=(
BOUNDED_CURVE()
B_SPLINE_CURVE(2,(#10187,#10188,#10189,#10190,#10191,#10192,#10193),
 .UNSPECIFIED.,.F.,.F.)
B_SPLINE_CURVE_WITH_KNOTS((3,2,2,3),(0.46070645710654,0.472222222222222,
0.486111111111111,0.498019907343005),.UNSPECIFIED.)
CURVE()
GEOMETRIC_REPRESENTATION_ITEM()
RATIONAL_B_SPLINE_CURVE((0.990345417239974,0.971747906970446,1.,0.965925826289068,
1.,0.970783667812457,0.991669449544642))
REPRESENTATION_ITEM('')
);
#243=(
BOUNDED_CURVE()
B_SPLINE_CURVE(2,(#10502,#10503,#10504,#10505,#10506,#10507,#10508),
 .UNSPECIFIED.,.F.,.F.)
B_SPLINE_CURVE_WITH_KNOTS((3,2,2,3),(0.669182585268271,0.680555555555556,
0.694444444444444,0.706339757525137),.UNSPECIFIED.)
CURVE()
GEOMETRIC_REPRESENTATION_ITEM()
RATIONAL_B_SPLINE_CURVE((0.989891404642439,0.97209823130717,1.,0.965925826289068,
1.,0.970816746573466,0.991622219962871))
REPRESENTATION_ITEM('')
);
#244=(
BOUNDED_CURVE()
B_SPLINE_CURVE(2,(#10518,#10519,#10520,#10521,#10522,#10523,#10524),
 .UNSPECIFIED.,.F.,.F.)
B_SPLINE_CURVE_WITH_KNOTS((3,2,2,3),(0.669043036225234,0.680555555555556,
0.694444444444444,0.706021829576019),.UNSPECIFIED.)
CURVE()
GEOMETRIC_REPRESENTATION_ITEM()
RATIONAL_B_SPLINE_CURVE((0.99033493732901,0.971755869987148,1.,0.965925826289068,
1.,0.971596732089403,0.990545786488669))
REPRESENTATION_ITEM('')
);
#245=(
BOUNDED_CURVE()
B_SPLINE_CURVE(2,(#10823,#10824,#10825,#10826,#10827,#10828,#10829),
 .UNSPECIFIED.,.F.,.F.)
B_SPLINE_CURVE_WITH_KNOTS((3,2,2,3),(0.627373123773207,0.638888888888889,
0.652777777777778,0.664686574009672),.UNSPECIFIED.)
CURVE()
GEOMETRIC_REPRESENTATION_ITEM()
RATIONAL_B_SPLINE_CURVE((0.990345417239974,0.971747906970446,1.,0.965925826289068,
1.,0.970783667812458,0.991669449544642))
REPRESENTATION_ITEM('')
);
#246=(
BOUNDED_CURVE()
B_SPLINE_CURVE(2,(#10841,#10842,#10843,#10844,#10845,#10846,#10847),
 .UNSPECIFIED.,.F.,.F.)
B_SPLINE_CURVE_WITH_KNOTS((3,2,2,3),(0.62751099544001,0.638888888888889,
0.652777777777778,0.664570329915933),.UNSPECIFIED.)
CURVE()
GEOMETRIC_REPRESENTATION_ITEM()
RATIONAL_B_SPLINE_CURVE((0.989906817917388,0.972086153115408,1.,0.965925826289068,
1.,0.971068854156347,0.991266482904706))
REPRESENTATION_ITEM('')
);
#247=(
BOUNDED_CURVE()
B_SPLINE_CURVE(2,(#10859,#10860,#10861,#10862,#10863,#10864,#10865),
 .UNSPECIFIED.,.F.,.F.)
B_SPLINE_CURVE_WITH_KNOTS((3,2,2,3),(0.0436499985776507,0.0555555555555556,
0.0694444444444444,0.0809569637747658),.UNSPECIFIED.)
CURVE()
GEOMETRIC_REPRESENTATION_ITEM()
RATIONAL_B_SPLINE_CURVE((0.991658091170858,0.970791614805482,1.,0.965925826289068,
1.,0.971755869987148,0.99033493732901))
REPRESENTATION_ITEM('')
);
#248=(
BOUNDED_CURVE()
B_SPLINE_CURVE(2,(#10872,#10873,#10874,#10875,#10876,#10877,#10878),
 .UNSPECIFIED.,.F.,.F.)
B_SPLINE_CURVE_WITH_KNOTS((3,2,2,3),(0.0853134259903282,0.0972222222222222,
0.111111111111111,0.123016668089016),.UNSPECIFIED.)
CURVE()
GEOMETRIC_REPRESENTATION_ITEM()
RATIONAL_B_SPLINE_CURVE((0.991669449544642,0.970783667812458,1.,0.965925826289068,
1.,0.970791614805482,0.991658091170858))
REPRESENTATION_ITEM('')
);
#249=(
BOUNDED_CURVE()
B_SPLINE_CURVE(2,(#10883,#10884,#10885,#10886,#10887,#10888,#10889),
 .UNSPECIFIED.,.F.,.F.)
B_SPLINE_CURVE_WITH_KNOTS((3,2,2,3),(0.210316665244317,0.222222222222222,
0.236111111111111,0.247623630441432),.UNSPECIFIED.)
CURVE()
GEOMETRIC_REPRESENTATION_ITEM()
RATIONAL_B_SPLINE_CURVE((0.991658091170858,0.970791614805482,1.,0.965925826289068,
1.,0.971755869987148,0.99033493732901))
REPRESENTATION_ITEM('')
);
#250=(
BOUNDED_CURVE()
B_SPLINE_CURVE(2,(#10896,#10897,#10898,#10899,#10900,#10901,#10902),
 .UNSPECIFIED.,.F.,.F.)
B_SPLINE_CURVE_WITH_KNOTS((3,2,2,3),(0.251980092656995,0.263888888888889,
0.277777777777778,0.289683334755683),.UNSPECIFIED.)
CURVE()
GEOMETRIC_REPRESENTATION_ITEM()
RATIONAL_B_SPLINE_CURVE((0.991669449544642,0.970783667812457,1.,0.965925826289068,
1.,0.970791614805482,0.991658091170858))
REPRESENTATION_ITEM('')
);
#251=(
BOUNDED_CURVE()
B_SPLINE_CURVE(2,(#10907,#10908,#10909,#10910,#10911,#10912,#10913),
 .UNSPECIFIED.,.F.,.F.)
B_SPLINE_CURVE_WITH_KNOTS((3,2,2,3),(0.376983331910984,0.388888888888889,
0.402777777777778,0.414290297108099),.UNSPECIFIED.)
CURVE()
GEOMETRIC_REPRESENTATION_ITEM()
RATIONAL_B_SPLINE_CURVE((0.991658091170857,0.970791614805482,1.,0.965925826289068,
1.,0.971755869987148,0.99033493732901))
REPRESENTATION_ITEM('')
);
#252=(
BOUNDED_CURVE()
B_SPLINE_CURVE(2,(#10920,#10921,#10922,#10923,#10924,#10925,#10926),
 .UNSPECIFIED.,.F.,.F.)
B_SPLINE_CURVE_WITH_KNOTS((3,2,2,3),(0.418646759323662,0.430555555555556,
0.444444444444444,0.456350001422349),.UNSPECIFIED.)
CURVE()
GEOMETRIC_REPRESENTATION_ITEM()
RATIONAL_B_SPLINE_CURVE((0.991669449544642,0.970783667812457,1.,0.965925826289068,
1.,0.970791614805482,0.991658091170858))
REPRESENTATION_ITEM('')
);
#253=(
BOUNDED_CURVE()
B_SPLINE_CURVE(2,(#10931,#10932,#10933,#10934,#10935,#10936,#10937),
 .UNSPECIFIED.,.F.,.F.)
B_SPLINE_CURVE_WITH_KNOTS((3,2,2,3),(0.543649998577651,0.555555555555556,
0.569444444444444,0.580956963774766),.UNSPECIFIED.)
CURVE()
GEOMETRIC_REPRESENTATION_ITEM()
RATIONAL_B_SPLINE_CURVE((0.991658091170858,0.970791614805482,1.,0.965925826289068,
1.,0.971755869987148,0.99033493732901))
REPRESENTATION_ITEM('')
);
#254=(
BOUNDED_CURVE()
B_SPLINE_CURVE(2,(#10944,#10945,#10946,#10947,#10948,#10949,#10950),
 .UNSPECIFIED.,.F.,.F.)
B_SPLINE_CURVE_WITH_KNOTS((3,2,2,3),(0.585313425990328,0.597222222222222,
0.611111111111111,0.623016668089016),.UNSPECIFIED.)
CURVE()
GEOMETRIC_REPRESENTATION_ITEM()
RATIONAL_B_SPLINE_CURVE((0.991669449544642,0.970783667812458,1.,0.965925826289068,
1.,0.970791614805482,0.991658091170858))
REPRESENTATION_ITEM('')
);
#255=(
BOUNDED_CURVE()
B_SPLINE_CURVE(2,(#10956,#10957,#10958,#10959,#10960,#10961,#10962),
 .UNSPECIFIED.,.F.,.F.)
B_SPLINE_CURVE_WITH_KNOTS((3,2,2,3),(0.00237636955856754,0.0138888888888889,
0.0277777777777778,0.0392935428934596),.UNSPECIFIED.)
CURVE()
GEOMETRIC_REPRESENTATION_ITEM()
RATIONAL_B_SPLINE_CURVE((0.99033493732901,0.971755869987148,1.,0.965925826289068,
1.,0.971747906970446,0.990345417239974))
REPRESENTATION_ITEM('')
);
#256=(
BOUNDED_CURVE()
B_SPLINE_CURVE(2,(#10968,#10969,#10970,#10971,#10972,#10973,#10974),
 .UNSPECIFIED.,.F.,.F.)
B_SPLINE_CURVE_WITH_KNOTS((3,2,2,3),(0.169043036225234,0.180555555555556,
0.194444444444444,0.205960209560126),.UNSPECIFIED.)
CURVE()
GEOMETRIC_REPRESENTATION_ITEM()
RATIONAL_B_SPLINE_CURVE((0.99033493732901,0.971755869987148,1.,0.965925826289068,
1.,0.971747906970446,0.990345417239974))
REPRESENTATION_ITEM('')
);
#257=(
BOUNDED_CURVE()
B_SPLINE_CURVE(2,(#10979,#10980,#10981,#10982,#10983,#10984,#10985),
 .UNSPECIFIED.,.F.,.F.)
B_SPLINE_CURVE_WITH_KNOTS((3,2,2,3),(0.127373123773207,0.138888888888889,
0.152777777777778,0.164686574009672),.UNSPECIFIED.)
CURVE()
GEOMETRIC_REPRESENTATION_ITEM()
RATIONAL_B_SPLINE_CURVE((0.990345417239974,0.971747906970446,1.,0.965925826289068,
1.,0.970783667812458,0.991669449544642))
REPRESENTATION_ITEM('')
);
#258=(
BOUNDED_CURVE()
B_SPLINE_CURVE(2,(#10992,#10993,#10994,#10995,#10996,#10997,#10998),
 .UNSPECIFIED.,.F.,.F.)
B_SPLINE_CURVE_WITH_KNOTS((3,2,2,3),(0.335709702891901,0.347222222222222,
0.361111111111111,0.372626876226793),.UNSPECIFIED.)
CURVE()
GEOMETRIC_REPRESENTATION_ITEM()
RATIONAL_B_SPLINE_CURVE((0.99033493732901,0.971755869987148,1.,0.965925826289068,
1.,0.971747906970446,0.990345417239974))
REPRESENTATION_ITEM('')
);
#259=(
BOUNDED_CURVE()
B_SPLINE_CURVE(2,(#11003,#11004,#11005,#11006,#11007,#11008,#11009),
 .UNSPECIFIED.,.F.,.F.)
B_SPLINE_CURVE_WITH_KNOTS((3,2,2,3),(0.294039790439874,0.305555555555556,
0.319444444444444,0.331353240676338),.UNSPECIFIED.)
CURVE()
GEOMETRIC_REPRESENTATION_ITEM()
RATIONAL_B_SPLINE_CURVE((0.990345417239974,0.971747906970446,1.,0.965925826289068,
1.,0.970783667812457,0.991669449544642))
REPRESENTATION_ITEM('')
);
#260=(
BOUNDED_CURVE()
B_SPLINE_CURVE(2,(#11016,#11017,#11018,#11019,#11020,#11021,#11022),
 .UNSPECIFIED.,.F.,.F.)
B_SPLINE_CURVE_WITH_KNOTS((3,2,2,3),(0.502376369558567,0.513888888888889,
0.527777777777778,0.53929354289346),.UNSPECIFIED.)
CURVE()
GEOMETRIC_REPRESENTATION_ITEM()
RATIONAL_B_SPLINE_CURVE((0.99033493732901,0.971755869987148,1.,0.965925826289068,
1.,0.971747906970446,0.990345417239974))
REPRESENTATION_ITEM('')
);
#261=(
BOUNDED_CURVE()
B_SPLINE_CURVE(2,(#11027,#11028,#11029,#11030,#11031,#11032,#11033),
 .UNSPECIFIED.,.F.,.F.)
B_SPLINE_CURVE_WITH_KNOTS((3,2,2,3),(0.46070645710654,0.472222222222222,
0.486111111111111,0.498019907343005),.UNSPECIFIED.)
CURVE()
GEOMETRIC_REPRESENTATION_ITEM()
RATIONAL_B_SPLINE_CURVE((0.990345417239974,0.971747906970446,1.,0.965925826289068,
1.,0.970783667812457,0.991669449544642))
REPRESENTATION_ITEM('')
);
#262=(
BOUNDED_CURVE()
B_SPLINE_CURVE(2,(#11040,#11041,#11042,#11043,#11044,#11045,#11046),
 .UNSPECIFIED.,.F.,.F.)
B_SPLINE_CURVE_WITH_KNOTS((3,2,2,3),(0.669043036225234,0.680555555555556,
0.694444444444444,0.705960209560126),.UNSPECIFIED.)
CURVE()
GEOMETRIC_REPRESENTATION_ITEM()
RATIONAL_B_SPLINE_CURVE((0.99033493732901,0.971755869987148,1.,0.965925826289068,
1.,0.971747906970446,0.990345417239974))
REPRESENTATION_ITEM('')
);
#263=(
BOUNDED_CURVE()
B_SPLINE_CURVE(2,(#11056,#11057,#11058,#11059,#11060,#11061,#11062),
 .UNSPECIFIED.,.F.,.F.)
B_SPLINE_CURVE_WITH_KNOTS((3,2,2,3),(0.627373123773207,0.638888888888889,
0.652777777777778,0.664686574009672),.UNSPECIFIED.)
CURVE()
GEOMETRIC_REPRESENTATION_ITEM()
RATIONAL_B_SPLINE_CURVE((0.990345417239974,0.971747906970446,1.,0.965925826289068,
1.,0.970783667812458,0.991669449544642))
REPRESENTATION_ITEM('')
);
#264=(
BOUNDED_CURVE()
B_SPLINE_CURVE(2,(#11068,#11069,#11070,#11071,#11072,#11073,#11074),
 .UNSPECIFIED.,.F.,.F.)
B_SPLINE_CURVE_WITH_KNOTS((3,2,2,3),(0.710316665244317,0.722222222222222,
0.736111111111111,0.747623630441432),.UNSPECIFIED.)
CURVE()
GEOMETRIC_REPRESENTATION_ITEM()
RATIONAL_B_SPLINE_CURVE((0.991658091170858,0.970791614805482,1.,0.965925826289068,
1.,0.971755869987148,0.99033493732901))
REPRESENTATION_ITEM('')
);
#265=(
BOUNDED_CURVE()
B_SPLINE_CURVE(2,(#11078,#11079,#11080,#11081,#11082,#11083,#11084),
 .UNSPECIFIED.,.F.,.F.)
B_SPLINE_CURVE_WITH_KNOTS((3,2,2,3),(0.710237354772895,0.722222222222222,
0.736111111111111,0.747623630441432),.UNSPECIFIED.)
CURVE()
GEOMETRIC_REPRESENTATION_ITEM()
RATIONAL_B_SPLINE_CURVE((0.991938323047677,0.970597039213297,1.,0.965925826289068,
1.,0.971755869987148,0.99033493732901))
REPRESENTATION_ITEM('')
);
#266=(
BOUNDED_CURVE()
B_SPLINE_CURVE(2,(#11094,#11095,#11096,#11097,#11098,#11099,#11100),
 .UNSPECIFIED.,.F.,.F.)
B_SPLINE_CURVE_WITH_KNOTS((3,2,2,3),(0.751980092656995,0.763888888888889,
0.777777777777778,0.790814625085749),.UNSPECIFIED.)
CURVE()
GEOMETRIC_REPRESENTATION_ITEM()
RATIONAL_B_SPLINE_CURVE((0.991669449544642,0.970783667812458,1.,0.965925826289068,
1.,0.968016174413341,0.996075776898402))
REPRESENTATION_ITEM('')
);
#267=(
BOUNDED_CURVE()
B_SPLINE_CURVE(2,(#11104,#11105,#11106,#11107,#11108,#11109,#11110),
 .UNSPECIFIED.,.F.,.F.)
B_SPLINE_CURVE_WITH_KNOTS((3,2,2,3),(0.751980092656995,0.763888888888889,
0.777777777777778,0.790051277060462),.UNSPECIFIED.)
CURVE()
GEOMETRIC_REPRESENTATION_ITEM()
RATIONAL_B_SPLINE_CURVE((0.991669449544642,0.970783667812458,1.,0.965925826289068,
1.,0.969888927044859,0.99299567954319))
REPRESENTATION_ITEM('')
);
#268=(
BOUNDED_CURVE()
B_SPLINE_CURVE(2,(#11738,#11739,#11740,#11741,#11742),.UNSPECIFIED.,.F.,
 .F.)
B_SPLINE_CURVE_WITH_KNOTS((3,2,3),(0.100045993303939,0.111111111111111,
0.122900233666328),.UNSPECIFIED.)
CURVE()
GEOMETRIC_REPRESENTATION_ITEM()
RATIONAL_B_SPLINE_CURVE((0.988961607054814,0.972853498266867,1.,0.971077268091095,
0.991254739061418))
REPRESENTATION_ITEM('')
);
#269=(
BOUNDED_CURVE()
B_SPLINE_CURVE(2,(#13879,#13880,#13881,#13882,#13883,#13884,#13885),
 .UNSPECIFIED.,.F.,.F.)
B_SPLINE_CURVE_WITH_KNOTS((3,2,2,3),(0.00238251257661542,0.0138888888888889,
0.0277777777777778,0.0392874082837476),.UNSPECIFIED.)
CURVE()
GEOMETRIC_REPRESENTATION_ITEM()
RATIONAL_B_SPLINE_CURVE((0.990315123280967,0.971770940902162,1.,0.965925826289068,
1.,0.971762957256948,0.990325616225644))
REPRESENTATION_ITEM('')
);
#270=(
BOUNDED_CURVE()
B_SPLINE_CURVE(2,(#16908,#16909,#16910,#16911,#16912,#16913,#16914,#16915,
#16916,#16917,#16918,#16919,#16920),.UNSPECIFIED.,.F.,.F.)
B_SPLINE_CURVE_WITH_KNOTS((3,2,2,2,2,2,3),(0.752096336750733,0.763888888888889,
0.777777777777778,0.791666666666667,0.805555555555556,0.819444444444444,
0.8312369965826),.UNSPECIFIED.)
CURVE()
GEOMETRIC_REPRESENTATION_ITEM()
RATIONAL_B_SPLINE_CURVE((0.991266482904706,0.971068854156347,1.,0.965925826289068,
1.,0.965925826289068,1.,0.965925826289068,1.,0.965925826289068,1.,0.971068854156347,
0.991266482904706))
REPRESENTATION_ITEM('')
);
#271=(
BOUNDED_CURVE()
B_SPLINE_CURVE(2,(#16923,#16924,#16925,#16926,#16927,#16928,#16929,#16930,
#16931,#16932,#16933,#16934,#16935),.UNSPECIFIED.,.F.,.F.)
B_SPLINE_CURVE_WITH_KNOTS((3,2,2,2,2,2,3),(0.9187630034174,0.930555555555556,
0.944444444444444,0.958333333333333,0.972222222222222,0.986111111111111,
0.997903663249267),.UNSPECIFIED.)
CURVE()
GEOMETRIC_REPRESENTATION_ITEM()
RATIONAL_B_SPLINE_CURVE((0.991266482904706,0.971068854156347,1.,0.965925826289068,
1.,0.965925826289068,1.,0.965925826289068,1.,0.965925826289068,1.,0.971068854156347,
0.991266482904706))
REPRESENTATION_ITEM('')
);
#272=(
BOUNDED_CURVE()
B_SPLINE_CURVE(2,(#16941,#16942,#16943,#16944,#16945,#16946,#16947),
 .UNSPECIFIED.,.F.,.F.)
B_SPLINE_CURVE_WITH_KNOTS((3,2,2,3),(0.876137334108343,0.888888888888889,
0.902777777777778,0.914150748065062),.UNSPECIFIED.)
CURVE()
GEOMETRIC_REPRESENTATION_ITEM()
RATIONAL_B_SPLINE_CURVE((0.994876443540461,0.968716094127271,1.,0.965925826289068,
1.,0.97209823130717,0.989891404642439))
REPRESENTATION_ITEM('')
);
#273=(
BOUNDED_CURVE()
B_SPLINE_CURVE(2,(#16965,#16966,#16967,#16968,#16969,#16970,#16971),
 .UNSPECIFIED.,.F.,.F.)
B_SPLINE_CURVE_WITH_KNOTS((3,2,2,3),(0.70986335383276,0.722222222222222,
0.736111111111111,0.747484081398396),.UNSPECIFIED.)
CURVE()
GEOMETRIC_REPRESENTATION_ITEM()
RATIONAL_B_SPLINE_CURVE((0.993319695194941,0.969679487557137,1.,0.965925826289068,
1.,0.97209823130717,0.989891404642439))
REPRESENTATION_ITEM('')
);
#274=(
BOUNDED_CURVE()
B_SPLINE_CURVE(2,(#16989,#16990,#16991,#16992,#16993,#16994,#16995),
 .UNSPECIFIED.,.F.,.F.)
B_SPLINE_CURVE_WITH_KNOTS((3,2,2,3),(0.835849251934938,0.847222222222222,
0.861111111111111,0.87338656566107),.UNSPECIFIED.)
CURVE()
GEOMETRIC_REPRESENTATION_ITEM()
RATIONAL_B_SPLINE_CURVE((0.989891404642439,0.97209823130717,1.,0.965925826289068,
1.,0.969884130108453,0.993003043077312))
REPRESENTATION_ITEM('')
);
#275=(
BOUNDED_CURVE()
B_SPLINE_CURVE(2,(#17000,#17001,#17002,#17003,#17004,#17005,#17006),
 .UNSPECIFIED.,.F.,.F.)
B_SPLINE_CURVE_WITH_KNOTS((3,2,2,3),(0.794135813030579,0.805555555555556,
0.819444444444444,0.8312369965826),.UNSPECIFIED.)
CURVE()
GEOMETRIC_REPRESENTATION_ITEM()
RATIONAL_B_SPLINE_CURVE((0.990038529153568,0.971983483081829,1.,0.965925826289068,
1.,0.971068854156347,0.991266482904706))
REPRESENTATION_ITEM('')
);
#276=(
BOUNDED_CURVE()
B_SPLINE_CURVE(2,(#17600,#17601,#17602,#17603,#17604,#17605,#17606),
 .UNSPECIFIED.,.F.,.F.)
B_SPLINE_CURVE_WITH_KNOTS((3,2,2,3),(0.792847371553036,0.805555555555556,
0.819444444444444,0.831353240676339),.UNSPECIFIED.)
CURVE()
GEOMETRIC_REPRESENTATION_ITEM()
RATIONAL_B_SPLINE_CURVE((0.994699154130647,0.968822497413832,1.,0.965925826289068,
1.,0.970783667812457,0.991669449544642))
REPRESENTATION_ITEM('')
);
#277=(
BOUNDED_CURVE()
B_SPLINE_CURVE(2,(#17945,#17946,#17947,#17948,#17949,#17950,#17951,#17952,
#17953,#17954,#17955,#17956,#17957),.UNSPECIFIED.,.F.,.F.)
B_SPLINE_CURVE_WITH_KNOTS((3,2,2,2,2,2,3),(0.835709702891901,0.847222222222222,
0.861111111111111,0.875,0.888888888888889,0.902777777777778,0.914290297108099),
 .UNSPECIFIED.)
CURVE()
GEOMETRIC_REPRESENTATION_ITEM()
RATIONAL_B_SPLINE_CURVE((0.99033493732901,0.971755869987148,1.,0.965925826289068,
1.,0.965925826289068,1.,0.965925826289068,1.,0.965925826289068,1.,0.971755869987148,
0.99033493732901))
REPRESENTATION_ITEM('')
);
#278=(
BOUNDED_CURVE()
B_SPLINE_CURVE(2,(#18274,#18275,#18276,#18277,#18278,#18279,#18280,#18281,
#18282,#18283,#18284),.UNSPECIFIED.,.F.,.F.)
B_SPLINE_CURVE_WITH_KNOTS((3,2,2,2,2,3),(0.918646759323661,0.930555555555556,
0.944444444444444,0.958333333333333,0.972222222222222,0.972937471698986),
 .UNSPECIFIED.)
CURVE()
GEOMETRIC_REPRESENTATION_ITEM()
RATIONAL_B_SPLINE_CURVE((0.991669449544642,0.970783667812457,1.,0.965925826289068,
1.,0.965925826289068,1.,0.965925826289068,1.,0.998245249485912,0.996671231123559))
REPRESENTATION_ITEM('')
);
#279=(
BOUNDED_CURVE()
B_SPLINE_CURVE(2,(#18310,#18311,#18312,#18313,#18314,#18315,#18316),
 .UNSPECIFIED.,.F.,.F.)
B_SPLINE_CURVE_WITH_KNOTS((3,2,2,3),(0.793632040812071,0.805555555555556,
0.819444444444444,0.831353240676339),.UNSPECIFIED.)
CURVE()
GEOMETRIC_REPRESENTATION_ITEM()
RATIONAL_B_SPLINE_CURVE((0.991721153062242,0.970747558291768,1.,0.965925826289068,
1.,0.970783667812457,0.991669449544642))
REPRESENTATION_ITEM('')
);
#280=(
BOUNDED_CURVE()
B_SPLINE_CURVE(2,(#18327,#18328,#18329,#18330,#18331,#18332,#18333,#18334,
#18335,#18336,#18337,#18338,#18339),.UNSPECIFIED.,.F.,.F.)
B_SPLINE_CURVE_WITH_KNOTS((3,2,2,2,2,2,3),(0.835709702891901,0.847222222222222,
0.861111111111111,0.875,0.888888888888889,0.902777777777778,0.914290297108099),
 .UNSPECIFIED.)
CURVE()
GEOMETRIC_REPRESENTATION_ITEM()
RATIONAL_B_SPLINE_CURVE((0.99033493732901,0.971755869987148,1.,0.965925826289068,
1.,0.965925826289068,1.,0.965925826289068,1.,0.965925826289068,1.,0.971755869987148,
0.99033493732901))
REPRESENTATION_ITEM('')
);
#281=(
BOUNDED_CURVE()
B_SPLINE_CURVE(2,(#18346,#18347,#18348,#18349,#18350,#18351,#18352,#18353,
#18354,#18355,#18356,#18357,#18358),.UNSPECIFIED.,.F.,.F.)
B_SPLINE_CURVE_WITH_KNOTS((3,2,2,2,2,2,3),(0.918646759323661,0.930555555555556,
0.944444444444444,0.958333333333333,0.972222222222222,0.986111111111111,
0.998105847682342),.UNSPECIFIED.)
CURVE()
GEOMETRIC_REPRESENTATION_ITEM()
RATIONAL_B_SPLINE_CURVE((0.991669449544642,0.970783667812457,1.,0.965925826289068,
1.,0.965925826289068,1.,0.965925826289068,1.,0.965925826289068,1.,0.970572826896762,
0.991973505068469))
REPRESENTATION_ITEM('')
);
#282=(
BOUNDED_CURVE()
B_SPLINE_CURVE(2,(#19357,#19358,#19359),.UNSPECIFIED.,.F.,.F.)
B_SPLINE_CURVE_WITH_KNOTS((3,3),(0.921063726766605,0.935093935184017),
 .UNSPECIFIED.)
CURVE()
GEOMETRIC_REPRESENTATION_ITEM()
RATIONAL_B_SPLINE_CURVE((1.,0.978200372800764,0.98429423173899))
REPRESENTATION_ITEM('')
);
#283=(
BOUNDED_CURVE()
B_SPLINE_CURVE(2,(#19364,#19365,#19366,#19367,#19368,#19369,#19370,#19371,
#19372),.UNSPECIFIED.,.F.,.F.)
B_SPLINE_CURVE_WITH_KNOTS((3,2,2,2,3),(0.921063722504592,0.942993811135654,
0.964923899766715,0.986853988397777,0.999999994829099),.UNSPECIFIED.)
CURVE()
GEOMETRIC_REPRESENTATION_ITEM()
RATIONAL_B_SPLINE_CURVE((1.,0.965925826289068,1.,0.965925826289068,1.,0.965925826289068,
1.,0.979574221606877,0.98363692686735))
REPRESENTATION_ITEM('')
);
#284=(
BOUNDED_CURVE()
B_SPLINE_CURVE(2,(#19377,#19378,#19379,#19380,#19381,#19382,#19383,#19384,
#19385,#19386,#19387,#19388,#19389,#19390,#19391,#19392,#19393,#19394,#19395,
#19396,#19397,#19398,#19399,#19400,#19401),.UNSPECIFIED.,.F.,.F.)
B_SPLINE_CURVE_WITH_KNOTS((3,2,2,2,2,2,2,2,2,2,2,2,3),(0.657902661976146,
0.679832750708684,0.701762839441223,0.723692928173761,0.745623016906299,
0.767553105638837,0.789483194371375,0.811413283103914,0.833343371836452,
0.85527346056899,0.877203549301528,0.899133638034066,0.921063726766605),
 .UNSPECIFIED.)
CURVE()
GEOMETRIC_REPRESENTATION_ITEM()
RATIONAL_B_SPLINE_CURVE((1.,0.965925826289068,1.,0.965925826289068,1.,0.965925826289068,
1.,0.965925826289068,1.,0.965925826289068,1.,0.965925826289068,1.,0.965925826289068,
1.,0.965925826289068,1.,0.965925826289068,1.,0.965925826289068,1.,0.965925826289068,
1.,0.965925826289068,1.))
REPRESENTATION_ITEM('')
);
#285=(
BOUNDED_CURVE()
B_SPLINE_CURVE(2,(#19402,#19403,#19404,#19405,#19406,#19407,#19408,#19409,
#19410,#19411,#19412,#19413,#19414,#19415,#19416,#19417,#19418,#19419,#19420,
#19421,#19422,#19423,#19424,#19425,#19426),.UNSPECIFIED.,.F.,.F.)
B_SPLINE_CURVE_WITH_KNOTS((3,2,2,2,2,2,2,2,2,2,2,2,3),(0.657902658931851,
0.679832747562913,0.701762836193975,0.723692924825036,0.745623013456098,
0.76755310208716,0.789483190718221,0.811413279349283,0.833343367980345,
0.855273456611407,0.877203545242468,0.89913363387353,0.921063722504592),
 .UNSPECIFIED.)
CURVE()
GEOMETRIC_REPRESENTATION_ITEM()
RATIONAL_B_SPLINE_CURVE((1.,0.965925826289068,1.,0.965925826289068,1.,0.965925826289068,
1.,0.965925826289068,1.,0.965925826289068,1.,0.965925826289068,1.,0.965925826289068,
1.,0.965925826289068,1.,0.965925826289068,1.,0.965925826289068,1.,0.965925826289068,
1.,0.965925826289068,1.))
REPRESENTATION_ITEM('')
);
#286=(
BOUNDED_CURVE()
B_SPLINE_CURVE(2,(#19431,#19432,#19433,#19434,#19435,#19436,#19437,#19438,
#19439,#19440,#19441,#19442,#19443,#19444,#19445,#19446,#19447,#19448,#19449,
#19450,#19451,#19452,#19453,#19454,#19455),.UNSPECIFIED.,.F.,.F.)
B_SPLINE_CURVE_WITH_KNOTS((3,2,2,2,2,2,2,2,2,2,2,2,3),(0.394741597185688,
0.416671685918226,0.438601774650764,0.460531863383302,0.48246195211584,
0.504392040848379,0.526322129580917,0.548252218313455,0.570182307045993,
0.592112395778531,0.61404248451107,0.635972573243608,0.657902661976146),
 .UNSPECIFIED.)
CURVE()
GEOMETRIC_REPRESENTATION_ITEM()
RATIONAL_B_SPLINE_CURVE((1.,0.965925826289068,1.,0.965925826289068,1.,0.965925826289068,
1.,0.965925826289068,1.,0.965925826289068,1.,0.965925826289068,1.,0.965925826289068,
1.,0.965925826289068,1.,0.965925826289068,1.,0.965925826289068,1.,0.965925826289068,
1.,0.965925826289068,1.))
REPRESENTATION_ITEM('')
);
#287=(
BOUNDED_CURVE()
B_SPLINE_CURVE(2,(#19456,#19457,#19458,#19459,#19460,#19461,#19462,#19463,
#19464,#19465,#19466,#19467,#19468,#19469,#19470,#19471,#19472,#19473,#19474,
#19475,#19476,#19477,#19478,#19479,#19480),.UNSPECIFIED.,.F.,.F.)
B_SPLINE_CURVE_WITH_KNOTS((3,2,2,2,2,2,2,2,2,2,2,2,3),(0.394741595359111,
0.416671683990172,0.438601772621234,0.460531861252296,0.482461949883358,
0.504392038514419,0.526322127145481,0.548252215776543,0.570182304407604,
0.592112393038666,0.614042481669728,0.63597257030079,0.657902658931851),
 .UNSPECIFIED.)
CURVE()
GEOMETRIC_REPRESENTATION_ITEM()
RATIONAL_B_SPLINE_CURVE((1.,0.965925826289068,1.,0.965925826289068,1.,0.965925826289068,
1.,0.965925826289068,1.,0.965925826289068,1.,0.965925826289068,1.,0.965925826289068,
1.,0.965925826289068,1.,0.965925826289068,1.,0.965925826289068,1.,0.965925826289068,
1.,0.965925826289068,1.))
REPRESENTATION_ITEM('')
);
#288=(
BOUNDED_CURVE()
B_SPLINE_CURVE(2,(#19486,#19487,#19488,#19489,#19490,#19491,#19492,#19493,
#19494,#19495,#19496,#19497,#19498),.UNSPECIFIED.,.F.,.F.)
B_SPLINE_CURVE_WITH_KNOTS((3,2,2,2,2,2,3),(0.,0.0219300886310617,0.0438601772621234,
0.0657902658931851,0.0877203545242468,0.109650443155309,0.13158053178637),
 .UNSPECIFIED.)
CURVE()
GEOMETRIC_REPRESENTATION_ITEM()
RATIONAL_B_SPLINE_CURVE((1.,0.965925826289068,1.,0.965925826289068,1.,0.965925826289068,
1.,0.965925826289068,1.,0.965925826289068,1.,0.965925826289068,1.))
REPRESENTATION_ITEM('')
);
#289=(
BOUNDED_CURVE()
B_SPLINE_CURVE(2,(#19501,#19502,#19503,#19504,#19505,#19506,#19507,#19508,
#19509,#19510,#19511,#19512,#19513),.UNSPECIFIED.,.F.,.F.)
B_SPLINE_CURVE_WITH_KNOTS((3,2,2,2,2,2,3),(0.,0.0219300887325382,0.0438601774650764,
0.0657902661976146,0.0877203549301528,0.109650443662691,0.131580532395229),
 .UNSPECIFIED.)
CURVE()
GEOMETRIC_REPRESENTATION_ITEM()
RATIONAL_B_SPLINE_CURVE((1.,0.965925826289068,1.,0.965925826289068,1.,0.965925826289068,
1.,0.965925826289068,1.,0.965925826289068,1.,0.965925826289068,1.))
REPRESENTATION_ITEM('')
);
#290=(
BOUNDED_CURVE()
B_SPLINE_CURVE(2,(#19847,#19848,#19849,#19850,#19851,#19852,#19853,#19854,
#19855,#19856,#19857,#19858,#19859,#19860,#19861,#19862,#19863,#19864,#19865,
#19866,#19867,#19868,#19869,#19870,#19871),.UNSPECIFIED.,.F.,.F.)
B_SPLINE_CURVE_WITH_KNOTS((3,2,2,2,2,2,2,2,2,2,2,2,3),(0.131580532395229,
0.153510621127767,0.175440709860306,0.197370798592844,0.219300887325382,
0.24123097605792,0.263161064790458,0.285091153522997,0.307021242255535,
0.328951330988073,0.350881419720611,0.372811508453149,0.394741597185688),
 .UNSPECIFIED.)
CURVE()
GEOMETRIC_REPRESENTATION_ITEM()
RATIONAL_B_SPLINE_CURVE((1.,0.965925826289068,1.,0.965925826289068,1.,0.965925826289068,
1.,0.965925826289068,1.,0.965925826289068,1.,0.965925826289068,1.,0.965925826289068,
1.,0.965925826289068,1.,0.965925826289068,1.,0.965925826289068,1.,0.965925826289068,
1.,0.965925826289068,1.))
REPRESENTATION_ITEM('')
);
#291=(
BOUNDED_CURVE()
B_SPLINE_CURVE(2,(#19872,#19873,#19874,#19875,#19876,#19877,#19878,#19879,
#19880,#19881,#19882,#19883,#19884,#19885,#19886,#19887,#19888,#19889,#19890,
#19891,#19892,#19893,#19894,#19895,#19896),.UNSPECIFIED.,.F.,.F.)
B_SPLINE_CURVE_WITH_KNOTS((3,2,2,2,2,2,2,2,2,2,2,2,3),(0.13158053178637,
0.153510620417432,0.175440709048494,0.197370797679555,0.219300886310617,
0.241230974941679,0.26316106357274,0.285091152203802,0.307021240834864,
0.328951329465926,0.350881418096987,0.372811506728049,0.394741595359111),
 .UNSPECIFIED.)
CURVE()
GEOMETRIC_REPRESENTATION_ITEM()
RATIONAL_B_SPLINE_CURVE((1.,0.965925826289068,1.,0.965925826289068,1.,0.965925826289068,
1.,0.965925826289068,1.,0.965925826289068,1.,0.965925826289068,1.,0.965925826289068,
1.,0.965925826289068,1.,0.965925826289068,1.,0.965925826289068,1.,0.965925826289068,
1.,0.965925826289068,1.))
REPRESENTATION_ITEM('')
);
#292=(
BOUNDED_CURVE()
B_SPLINE_CURVE(2,(#20498,#20499,#20500),.UNSPECIFIED.,.F.,.F.)
B_SPLINE_CURVE_WITH_KNOTS((3,3),(0.0183343553427957,0.042559607390491),
 .UNSPECIFIED.)
CURVE()
GEOMETRIC_REPRESENTATION_ITEM()
RATIONAL_B_SPLINE_CURVE((1.12800823010849,1.2118132350172,1.29359962909812))
REPRESENTATION_ITEM('')
);
#293=(
BOUNDED_CURVE()
B_SPLINE_CURVE(2,(#20503,#20504,#20505),.UNSPECIFIED.,.F.,.F.)
B_SPLINE_CURVE_WITH_KNOTS((3,3),(-0.061743756665462,-0.0265578055647394),
 .UNSPECIFIED.)
CURVE()
GEOMETRIC_REPRESENTATION_ITEM()
RATIONAL_B_SPLINE_CURVE((1.28203378876711,1.20432016972132,1.12358878740287))
REPRESENTATION_ITEM('')
);
#294=B_SPLINE_CURVE_WITH_KNOTS('',3,(#5030,#5031,#5032,#5033,#5034,#5035,
#5036,#5037,#5038,#5039,#5040,#5041,#5042,#5043),.UNSPECIFIED.,.F.,.F.,
(4,2,2,2,2,2,4),(-1.03917131396603,-0.897633242543498,-0.747971508363487,
-0.598309774183476,-0.448752618812303,-0.299195463441129,-0.15765582292854),
 .UNSPECIFIED.);
#295=B_SPLINE_CURVE_WITH_KNOTS('',3,(#5051,#5052,#5053,#5054,#5055,#5056,
#5057,#5058,#5059,#5060,#5061,#5062,#5063,#5064),.UNSPECIFIED.,.F.,.F.,
(4,2,2,2,2,2,4),(0.15765582292854,0.299195463441129,0.448752618812303,0.598309774183476,
0.747971508363487,0.897633242543498,1.03917131396603),.UNSPECIFIED.);
#296=B_SPLINE_CURVE_WITH_KNOTS('',3,(#5068,#5069,#5070,#5071,#5072,#5073,
#5074,#5075,#5076,#5077,#5078,#5079,#5080,#5081,#5082,#5083,#5084,#5085),
 .UNSPECIFIED.,.F.,.F.,(4,2,2,2,2,2,2,2,4),(9.99999990605937E-7,1.61032997746592,
3.21316436538662,5.0051599487382,6.82527051959712,8.64573442526924,10.4385724656072,
12.0409045434925,13.6509631821543),.UNSPECIFIED.);
#297=B_SPLINE_CURVE_WITH_KNOTS('',3,(#5091,#5092,#5093,#5094,#5095,#5096),
 .UNSPECIFIED.,.F.,.F.,(4,2,4),(0.,0.149581313593702,0.157659940647757),
 .UNSPECIFIED.);
#298=B_SPLINE_CURVE_WITH_KNOTS('',3,(#5101,#5102,#5103,#5104,#5105,#5106,
#5107,#5108,#5109,#5110,#5111,#5112,#5113,#5114,#5115,#5116,#5117,#5118),
 .UNSPECIFIED.,.F.,.F.,(4,2,2,2,2,2,2,2,4),(-1.19705479780107,-1.04741995877816,
-0.89778511975524,-0.748086035420359,-0.598386951085478,-0.448814985396906,
-0.299243019708333,-0.149621509854167,0.),.UNSPECIFIED.);
#299=B_SPLINE_CURVE_WITH_KNOTS('',3,(#5126,#5127,#5128,#5129,#5130,#5131,
#5132,#5133,#5134,#5135,#5136,#5137,#5138,#5139,#5140,#5141,#5142,#5143),
 .UNSPECIFIED.,.F.,.F.,(4,2,2,2,2,2,2,2,4),(0.,0.149634938642595,0.299269877285189,
0.448970279983913,0.598670682682636,0.748241851215363,0.897813019748089,
1.04743440734167,1.19705579493525),.UNSPECIFIED.);
#300=B_SPLINE_CURVE_WITH_KNOTS('',3,(#5151,#5152,#5153,#5154,#5155,#5156,
#5157,#5158,#5159,#5160,#5161,#5162),.UNSPECIFIED.,.F.,.F.,(4,2,2,2,2,4),
(1.19705479780107,1.34668963682399,1.4963244758469,1.64602356018178,1.79572264451666,
1.83085170358366),.UNSPECIFIED.);
#301=B_SPLINE_CURVE_WITH_KNOTS('',3,(#5167,#5168,#5169,#5170,#5171,#5172,
#5173,#5174,#5175,#5176),.UNSPECIFIED.,.F.,.F.,(4,2,2,2,4),(1.83085170358366,
1.94529461020524,2.09486657589381,2.24448808574798,2.39410959560214),
 .UNSPECIFIED.);
#302=B_SPLINE_CURVE_WITH_KNOTS('',3,(#5184,#5185,#5186,#5187,#5188,#5189,
#5190,#5191,#5192,#5193,#5194,#5195,#5196,#5197,#5198,#5199,#5200,#5201),
 .UNSPECIFIED.,.F.,.F.,(4,2,2,2,2,2,2,2,4),(1.19705579493525,1.34667718252883,
1.49629857012241,1.64586973865514,1.79544090718787,1.94514130988659,2.09484171258531,
2.24447665122791,2.3941115898705),.UNSPECIFIED.);
#303=B_SPLINE_CURVE_WITH_KNOTS('',3,(#5241,#5242,#5243,#5244),
 .UNSPECIFIED.,.F.,.F.,(4,4),(-0.0621119208606391,-0.00070906240656004),
 .UNSPECIFIED.);
#304=B_SPLINE_CURVE_WITH_KNOTS('',3,(#5840,#5841,#5842,#5843,#5844,#5845,
#5846),.UNSPECIFIED.,.F.,.F.,(4,1,2,4),(6.93889390390723E-18,0.000802008422543448,
0.00160401684508564,0.00313358895216332),.UNSPECIFIED.);
#305=B_SPLINE_CURVE_WITH_KNOTS('',3,(#6138,#6139,#6140,#6141,#6142,#6143,
#6144),.UNSPECIFIED.,.F.,.F.,(4,1,2,4),(6.93889390390723E-18,0.000802008422543318,
0.00160401684508542,0.00313356353166787),.UNSPECIFIED.);
#306=B_SPLINE_CURVE_WITH_KNOTS('',3,(#6153,#6154,#6155,#6156,#6157,#6158,
#6159,#6160,#6161),.UNSPECIFIED.,.F.,.F.,(4,2,3,4),(0.,0.000802008422906776,
0.00160401684587021,0.00313013376960514),.UNSPECIFIED.);
#307=B_SPLINE_CURVE_WITH_KNOTS('',3,(#6462,#6463,#6464,#6465,#6466,#6467,
#6468),.UNSPECIFIED.,.F.,.F.,(4,1,2,4),(0.,0.000802008422543473,0.00160401684508569,
0.0031335889521633),.UNSPECIFIED.);
#308=B_SPLINE_CURVE_WITH_KNOTS('',3,(#6760,#6761,#6762,#6763,#6764,#6765,
#6766),.UNSPECIFIED.,.F.,.F.,(4,1,2,4),(1.55158384577955E-17,0.000802008422543312,
0.0016040168450854,0.00313356353166786),.UNSPECIFIED.);
#309=B_SPLINE_CURVE_WITH_KNOTS('',3,(#6775,#6776,#6777,#6778,#6779,#6780,
#6781,#6782,#6783),.UNSPECIFIED.,.F.,.F.,(4,2,3,4),(0.,0.000802008422906776,
0.0016040168458702,0.00313013376960513),.UNSPECIFIED.);
#310=B_SPLINE_CURVE_WITH_KNOTS('',3,(#7084,#7085,#7086,#7087,#7088,#7089,
#7090),.UNSPECIFIED.,.F.,.F.,(4,1,2,4),(0.,0.000802008422543476,0.00160401684508569,
0.00313358895216332),.UNSPECIFIED.);
#311=B_SPLINE_CURVE_WITH_KNOTS('',3,(#7382,#7383,#7384,#7385,#7386,#7387,
#7388),.UNSPECIFIED.,.F.,.F.,(4,1,2,4),(1.55158384577955E-17,0.000802008422543312,
0.0016040168450854,0.00313356353166786),.UNSPECIFIED.);
#312=B_SPLINE_CURVE_WITH_KNOTS('',3,(#7397,#7398,#7399,#7400,#7401,#7402,
#7403,#7404,#7405),.UNSPECIFIED.,.F.,.F.,(4,2,3,4),(0.,0.000802008422906761,
0.0016040168458702,0.00313013376960514),.UNSPECIFIED.);
#313=B_SPLINE_CURVE_WITH_KNOTS('',3,(#7706,#7707,#7708,#7709,#7710,#7711,
#7712),.UNSPECIFIED.,.F.,.F.,(4,1,2,4),(6.93889390390723E-18,0.000802008422543454,
0.00160401684508567,0.00313358895216332),.UNSPECIFIED.);
#314=B_SPLINE_CURVE_WITH_KNOTS('',3,(#8004,#8005,#8006,#8007,#8008,#8009,
#8010),.UNSPECIFIED.,.F.,.F.,(4,1,2,4),(6.93889390390723E-18,0.000802008422543302,
0.00160401684508539,0.00313356353166788),.UNSPECIFIED.);
#315=B_SPLINE_CURVE_WITH_KNOTS('',3,(#8020,#8021,#8022,#8023,#8024,#8025,
#8026,#8027,#8028,#8029),.UNSPECIFIED.,.F.,.F.,(4,3,3,4),(0.,0.00080200842290677,
0.00160401684587019,0.00311589056383513),.UNSPECIFIED.);
#316=B_SPLINE_CURVE_WITH_KNOTS('',3,(#8322,#8323,#8324,#8325,#8326,#8327,
#8328),.UNSPECIFIED.,.F.,.F.,(4,1,2,4),(9.81307786677359E-18,0.000802008422577623,
0.00160401684514919,0.00290160460940762),.UNSPECIFIED.);
#317=B_SPLINE_CURVE_WITH_KNOTS('',3,(#8635,#8636,#8637,#8638,#8639,#8640,
#8641),.UNSPECIFIED.,.F.,.F.,(4,1,2,4),(6.93889390390723E-18,0.000802008422577624,
0.00160401684514921,0.00313695506663807),.UNSPECIFIED.);
#318=B_SPLINE_CURVE_WITH_KNOTS('',3,(#8950,#8951,#8952,#8953,#8954,#8955,
#8956,#8957,#8958),.UNSPECIFIED.,.F.,.F.,(4,2,3,4),(0.,0.000802008422904874,
0.00160401684586611,0.00313011409353478),.UNSPECIFIED.);
#319=B_SPLINE_CURVE_WITH_KNOTS('',3,(#8959,#8960,#8961,#8962,#8963,#8964,
#8965),.UNSPECIFIED.,.F.,.F.,(4,1,2,4),(0.,0.000802008422577178,0.00160401684514837,
0.00313692497239048),.UNSPECIFIED.);
#320=B_SPLINE_CURVE_WITH_KNOTS('',3,(#9257,#9258,#9259,#9260,#9261,#9262,
#9263),.UNSPECIFIED.,.F.,.F.,(4,1,2,4),(6.93889390390723E-18,0.000802008422577621,
0.00160401684514922,0.00313695506663807),.UNSPECIFIED.);
#321=B_SPLINE_CURVE_WITH_KNOTS('',3,(#9572,#9573,#9574,#9575,#9576,#9577,
#9578,#9579,#9580),.UNSPECIFIED.,.F.,.F.,(4,2,3,4),(0.,0.000802008422904867,
0.00160401684586611,0.00313011409353478),.UNSPECIFIED.);
#322=B_SPLINE_CURVE_WITH_KNOTS('',3,(#9581,#9582,#9583,#9584,#9585,#9586,
#9587),.UNSPECIFIED.,.F.,.F.,(4,1,2,4),(0.,0.000802008422577179,0.00160401684514836,
0.0031369249723905),.UNSPECIFIED.);
#323=B_SPLINE_CURVE_WITH_KNOTS('',3,(#9879,#9880,#9881,#9882,#9883,#9884,
#9885),.UNSPECIFIED.,.F.,.F.,(4,1,2,4),(0.,0.000802008422577639,0.00160401684514923,
0.00313695506663809),.UNSPECIFIED.);
#324=B_SPLINE_CURVE_WITH_KNOTS('',3,(#10194,#10195,#10196,#10197,#10198,
#10199,#10200,#10201,#10202),.UNSPECIFIED.,.F.,.F.,(4,2,3,4),(0.,0.000802008422904871,
0.0016040168458661,0.00313011409353478),.UNSPECIFIED.);
#325=B_SPLINE_CURVE_WITH_KNOTS('',3,(#10203,#10204,#10205,#10206,#10207,
#10208,#10209),.UNSPECIFIED.,.F.,.F.,(4,1,2,4),(0.,0.000802008422577185,
0.00160401684514837,0.00313692497239049),.UNSPECIFIED.);
#326=B_SPLINE_CURVE_WITH_KNOTS('',3,(#10510,#10511,#10512,#10513,#10514,
#10515,#10516),.UNSPECIFIED.,.F.,.F.,(4,1,2,4),(0.,0.000802008422577623,
0.0016040168451492,0.00313695506663806),.UNSPECIFIED.);
#327=B_SPLINE_CURVE_WITH_KNOTS('',3,(#10525,#10526,#10527,#10528,#10529,
#10530),.UNSPECIFIED.,.F.,.F.,(4,2,4),(-0.317506811553133,-0.158581801084095,
0.),.UNSPECIFIED.);
#328=B_SPLINE_CURVE_WITH_KNOTS('',3,(#10831,#10832,#10833,#10834,#10835,
#10836,#10837,#10838,#10839),.UNSPECIFIED.,.F.,.F.,(4,2,3,4),(0.,0.000802008422904858,
0.00160401684586608,0.00313011409353478),.UNSPECIFIED.);
#329=B_SPLINE_CURVE_WITH_KNOTS('',3,(#10850,#10851,#10852,#10853,#10854,
#10855),.UNSPECIFIED.,.F.,.F.,(4,2,4),(1.31690409731013E-6,0.127022192229024,
0.28504745144389),.UNSPECIFIED.);
#330=B_SPLINE_CURVE_WITH_KNOTS('',3,(#11049,#11050,#11051,#11052),
 .UNSPECIFIED.,.F.,.F.,(4,4),(2.66453525910035E-15,0.0918230658993515),
 .UNSPECIFIED.);
#331=B_SPLINE_CURVE_WITH_KNOTS('',3,(#11086,#11087,#11088,#11089),
 .UNSPECIFIED.,.F.,.F.,(4,4),(1.09261755714425,1.19656563806167),
 .UNSPECIFIED.);
#332=B_SPLINE_CURVE_WITH_KNOTS('',3,(#11111,#11112,#11113,#11114,#11115,
#11116),.UNSPECIFIED.,.F.,.F.,(4,2,4),(-0.972867842394702,-0.897435512998064,
-0.788327277048526),.UNSPECIFIED.);
#333=B_SPLINE_CURVE_WITH_KNOTS('',3,(#11409,#11410,#11411,#11412,#11413,
#11414,#11415,#11416,#11417,#11418,#11419,#11420),.UNSPECIFIED.,.F.,.F.,
(4,2,2,2,2,4),(1.00000000158624E-6,0.692107157618177,1.39024716069207,2.74744494620693,
4.13283236453521,5.48383660931837),.UNSPECIFIED.);
#334=B_SPLINE_CURVE_WITH_KNOTS('',3,(#11421,#11422,#11423,#11424,#11425,
#11426),.UNSPECIFIED.,.F.,.F.,(4,2,4),(0.00114961664817087,0.0016040168451492,
0.00313695506663806),.UNSPECIFIED.);
#335=B_SPLINE_CURVE_WITH_KNOTS('',3,(#11721,#11722,#11723,#11724,#11725,
#11726,#11727,#11728,#11729),.UNSPECIFIED.,.F.,.F.,(4,2,3,4),(0.,0.000802008422904852,
0.00160401684586607,0.00224980714452562),.UNSPECIFIED.);
#336=B_SPLINE_CURVE_WITH_KNOTS('',3,(#11731,#11732,#11733,#11734,#11735,
#11736),.UNSPECIFIED.,.F.,.F.,(4,2,4),(1.00000000468185E-6,1.2811788104379,
2.56201318882656),.UNSPECIFIED.);
#337=B_SPLINE_CURVE_WITH_KNOTS('',3,(#11743,#11744,#11745,#11746,#11747,
#11748,#11749),.UNSPECIFIED.,.F.,.F.,(4,1,2,4),(0.,0.000802008422543476,
0.00160401684508567,0.00313358895216331),.UNSPECIFIED.);
#338=B_SPLINE_CURVE_WITH_KNOTS('',3,(#12040,#12041,#12042,#12043,#12044,
#12045,#12046),.UNSPECIFIED.,.F.,.F.,(4,1,2,4),(0.,0.000802008422577623,
0.00160401684514919,0.00313695506663806),.UNSPECIFIED.);
#339=B_SPLINE_CURVE_WITH_KNOTS('',3,(#12047,#12048,#12049,#12050,#12051,
#12052,#12053,#12054,#12055),.UNSPECIFIED.,.F.,.F.,(4,2,3,4),(0.,0.000802008422906758,
0.00160401684587019,0.00313013376960513),.UNSPECIFIED.);
#340=B_SPLINE_CURVE_WITH_KNOTS('',3,(#12346,#12347,#12348,#12349,#12350,
#12351,#12352,#12353,#12354),.UNSPECIFIED.,.F.,.F.,(4,2,3,4),(0.,0.000802008422904855,
0.00160401684586608,0.00313011409353478),.UNSPECIFIED.);
#341=B_SPLINE_CURVE_WITH_KNOTS('',3,(#12355,#12356,#12357,#12358,#12359,
#12360,#12361),.UNSPECIFIED.,.F.,.F.,(4,1,2,4),(9.81307786677359E-18,0.000802008422543473,
0.00160401684508569,0.0031335889521633),.UNSPECIFIED.);
#342=B_SPLINE_CURVE_WITH_KNOTS('',3,(#12652,#12653,#12654,#12655,#12656,
#12657,#12658),.UNSPECIFIED.,.F.,.F.,(4,1,2,4),(0.,0.000802008422577623,
0.0016040168451492,0.00313695506663807),.UNSPECIFIED.);
#343=B_SPLINE_CURVE_WITH_KNOTS('',3,(#12659,#12660,#12661,#12662,#12663,
#12664,#12665,#12666,#12667),.UNSPECIFIED.,.F.,.F.,(4,2,3,4),(0.,0.000802008422906776,
0.00160401684587021,0.00313013376960513),.UNSPECIFIED.);
#344=B_SPLINE_CURVE_WITH_KNOTS('',3,(#12958,#12959,#12960,#12961,#12962,
#12963,#12964,#12965,#12966),.UNSPECIFIED.,.F.,.F.,(4,2,3,4),(0.,0.000802008422904862,
0.00160401684586608,0.00313011409353477),.UNSPECIFIED.);
#345=B_SPLINE_CURVE_WITH_KNOTS('',3,(#12967,#12968,#12969,#12970,#12971,
#12972,#12973),.UNSPECIFIED.,.F.,.F.,(4,1,2,4),(6.93889390390723E-18,0.000802008422543466,
0.00160401684508568,0.00313358895216331),.UNSPECIFIED.);
#346=B_SPLINE_CURVE_WITH_KNOTS('',3,(#13264,#13265,#13266,#13267,#13268,
#13269,#13270),.UNSPECIFIED.,.F.,.F.,(4,1,2,4),(0.,0.00080200842257763,
0.0016040168451492,0.00313695506663807),.UNSPECIFIED.);
#347=B_SPLINE_CURVE_WITH_KNOTS('',3,(#13271,#13272,#13273,#13274,#13275,
#13276,#13277,#13278,#13279),.UNSPECIFIED.,.F.,.F.,(4,2,3,4),(0.,0.000802008422906769,
0.0016040168458702,0.00313013376960513),.UNSPECIFIED.);
#348=B_SPLINE_CURVE_WITH_KNOTS('',3,(#13570,#13571,#13572,#13573,#13574,
#13575,#13576,#13577,#13578),.UNSPECIFIED.,.F.,.F.,(4,2,3,4),(0.,0.000802008422904853,
0.00160401684586608,0.00313011409353477),.UNSPECIFIED.);
#349=B_SPLINE_CURVE_WITH_KNOTS('',3,(#13579,#13580,#13581,#13582,#13583,
#13584,#13585),.UNSPECIFIED.,.F.,.F.,(4,1,2,4),(0.,0.000802008422543461,
0.00160401684508566,0.00313358895216331),.UNSPECIFIED.);
#350=B_SPLINE_CURVE_WITH_KNOTS('',3,(#14178,#14179,#14180,#14181,#14182,
#14183,#14184),.UNSPECIFIED.,.F.,.F.,(4,1,2,4),(6.93889390390723E-18,0.000802008422577189,
0.00160401684514838,0.00313692497239048),.UNSPECIFIED.);
#351=B_SPLINE_CURVE_WITH_KNOTS('',3,(#14475,#14476,#14477,#14478,#14479,
#14480,#14481),.UNSPECIFIED.,.F.,.F.,(4,1,2,4),(0.,0.000802008422543314,
0.0016040168450854,0.00313356353166786),.UNSPECIFIED.);
#352=B_SPLINE_CURVE_WITH_KNOTS('',3,(#14774,#14775,#14776,#14777,#14778,
#14779,#14780),.UNSPECIFIED.,.F.,.F.,(4,1,2,4),(0.,0.000802008422577183,
0.00160401684514837,0.00313692497239049),.UNSPECIFIED.);
#353=B_SPLINE_CURVE_WITH_KNOTS('',3,(#15071,#15072,#15073,#15074,#15075,
#15076,#15077),.UNSPECIFIED.,.F.,.F.,(4,1,2,4),(0.,0.000802008422543321,
0.0016040168450854,0.00313356353166786),.UNSPECIFIED.);
#354=B_SPLINE_CURVE_WITH_KNOTS('',3,(#15370,#15371,#15372,#15373,#15374,
#15375,#15376),.UNSPECIFIED.,.F.,.F.,(4,1,2,4),(9.81307786677359E-18,0.000802008422577179,
0.00160401684514837,0.0031369249723905),.UNSPECIFIED.);
#355=B_SPLINE_CURVE_WITH_KNOTS('',3,(#15667,#15668,#15669,#15670,#15671,
#15672,#15673),.UNSPECIFIED.,.F.,.F.,(4,1,2,4),(0.,0.00080200842254332,
0.0016040168450854,0.00313356353166787),.UNSPECIFIED.);
#356=B_SPLINE_CURVE_WITH_KNOTS('',3,(#15966,#15967,#15968,#15969,#15970,
#15971,#15972),.UNSPECIFIED.,.F.,.F.,(4,1,2,4),(0.,0.000802008422577182,
0.00160401684514837,0.00313692497239049),.UNSPECIFIED.);
#357=B_SPLINE_CURVE_WITH_KNOTS('',3,(#16263,#16264,#16265,#16266,#16267,
#16268,#16269),.UNSPECIFIED.,.F.,.F.,(4,1,2,4),(0.,0.000802008422543311,
0.00160401684508539,0.00313356353166786),.UNSPECIFIED.);
#358=B_SPLINE_CURVE_WITH_KNOTS('',3,(#16561,#16562,#16563,#16564,#16565,
#16566,#16567),.UNSPECIFIED.,.F.,.F.,(4,1,2,4),(0.,0.000802008422577623,
0.0016040168451492,0.00313695506663805),.UNSPECIFIED.);
#359=B_SPLINE_CURVE_WITH_KNOTS('',3,(#16568,#16569,#16570,#16571,#16572,
#16573,#16574,#16575,#16576),.UNSPECIFIED.,.F.,.F.,(4,2,3,4),(0.,0.000802008422906782,
0.00160401684587023,0.00313013376960512),.UNSPECIFIED.);
#360=B_SPLINE_CURVE_WITH_KNOTS('',3,(#16867,#16868,#16869,#16870,#16871,
#16872,#16873,#16874,#16875),.UNSPECIFIED.,.F.,.F.,(4,2,3,4),(0.,0.000802008422904849,
0.00160401684586607,0.00313011409353477),.UNSPECIFIED.);
#361=B_SPLINE_CURVE_WITH_KNOTS('',3,(#16876,#16877,#16878,#16879,#16880,
#16881),.UNSPECIFIED.,.F.,.F.,(4,2,4),(-0.322960607525434,-0.161416672138243,
0.),.UNSPECIFIED.);
#362=B_SPLINE_CURVE_WITH_KNOTS('',3,(#16949,#16950,#16951,#16952,#16953,
#16954,#16955,#16956,#16957,#16958,#16959,#16960,#16961,#16962,#16963,#16964),
 .UNSPECIFIED.,.F.,.F.,(4,3,3,3,3,4),(0.00869267220315778,0.00897347831546948,
0.00914767037620121,0.00934133695348868,0.00953512469214104,0.00960266854924464),
 .UNSPECIFIED.);
#363=B_SPLINE_CURVE_WITH_KNOTS('',3,(#16976,#16977,#16978,#16979,#16980,
#16981,#16982,#16983,#16984,#16985,#16986,#16987,#16988),.UNSPECIFIED.,
 .F.,.F.,(4,3,3,3,4),(0.014648624615312,0.0149251039211043,0.0151052218084313,
0.0153888521719278,0.0155618190015507),.UNSPECIFIED.);
#364=B_SPLINE_CURVE_WITH_KNOTS('',3,(#17007,#17008,#17009,#17010),
 .UNSPECIFIED.,.F.,.F.,(4,4),(-1.18244232933534,-1.12154327892906),
 .UNSPECIFIED.);
#365=B_SPLINE_CURVE_WITH_KNOTS('',3,(#17302,#17303,#17304,#17305,#17306,
#17307),.UNSPECIFIED.,.F.,.F.,(4,2,4),(-0.319108104097769,-0.159717462303668,
0.),.UNSPECIFIED.);
#366=B_SPLINE_CURVE_WITH_KNOTS('',3,(#17607,#17608,#17609,#17610,#17611,
#17612,#17613,#17614,#17615),.UNSPECIFIED.,.F.,.F.,(4,2,3,4),(0.,0.000802008422904865,
0.00160401684586611,0.00313011409353478),.UNSPECIFIED.);
#367=B_SPLINE_CURVE_WITH_KNOTS('',3,(#17616,#17617,#17618,#17619,#17620,
#17621,#17622),.UNSPECIFIED.,.F.,.F.,(4,1,2,4),(6.93889390390723E-18,0.000802008422543296,
0.00160401684508538,0.00313356353166788),.UNSPECIFIED.);
#368=B_SPLINE_CURVE_WITH_KNOTS('',3,(#17623,#17624,#17625,#17626,#17627,
#17628,#17629,#17630,#17631,#17632,#17633,#17634,#17635,#17636,#17637,#17638,
#17639,#17640,#17641,#17642,#17643,#17644,#17645,#17646,#17647,#17648,#17649,
#17650,#17651,#17652),.UNSPECIFIED.,.F.,.F.,(4,2,2,2,2,2,2,2,2,2,2,2,2,
2,4),(-0.422102272244324,-0.348146080556318,-0.281817985962111,-0.236711761741135,
-0.211595144460982,-0.211065138953951,-0.210876177667938,-0.210727417561504,
-0.210584548895218,-0.210388827790948,-0.209942749411974,-0.197138882545824,
-0.161673269341594,-0.105103214837917,0.),.UNSPECIFIED.);
#369=B_SPLINE_CURVE_WITH_KNOTS('',3,(#17960,#17961,#17962,#17963,#17964,
#17965),.UNSPECIFIED.,.F.,.F.,(4,2,4),(-0.280439425813684,-0.140217859912255,
0.),.UNSPECIFIED.);
#370=B_SPLINE_CURVE_WITH_KNOTS('',3,(#17966,#17967,#17968,#17969,#17970,
#17971,#17972),.UNSPECIFIED.,.F.,.F.,(4,1,2,4),(0.,0.00080200842257764,
0.00160401684514921,0.00313695506663809),.UNSPECIFIED.);
#371=B_SPLINE_CURVE_WITH_KNOTS('',3,(#18265,#18266,#18267,#18268,#18269,
#18270),.UNSPECIFIED.,.F.,.F.,(4,2,4),(-0.30638474699579,-0.153201892366487,
-9.99999968504403E-7),.UNSPECIFIED.);
#372=B_SPLINE_CURVE_WITH_KNOTS('',3,(#18286,#18287,#18288,#18289,#18290,
#18291,#18292,#18293,#18294,#18295,#18296,#18297,#18298,#18299,#18300,#18301,
#18302,#18303,#18304,#18305),.UNSPECIFIED.,.F.,.F.,(4,2,2,2,2,2,2,2,2,4),
(0.,0.623255442251575,1.23190737214536,2.44539704217141,2.79680652222767,
4.64794122889589,5.57465586747308,7.36134291536557,7.84478465660949,9.2535573537906),
 .UNSPECIFIED.);
#373=B_SPLINE_CURVE_WITH_KNOTS('',3,(#18318,#18319,#18320,#18321,#18322,
#18323),.UNSPECIFIED.,.F.,.F.,(4,2,4),(-0.420375087827024,-0.299144304587487,
-0.235961611475371),.UNSPECIFIED.);
#374=B_SPLINE_CURVE_WITH_KNOTS('',3,(#18360,#18361,#18362,#18363,#18364,
#18365),.UNSPECIFIED.,.F.,.F.,(4,2,4),(0.108137927283078,0.149564996746846,
0.157637941980081),.UNSPECIFIED.);
#375=B_SPLINE_CURVE_WITH_KNOTS('',3,(#18657,#18658,#18659,#18660,#18661,
#18662,#18663),.UNSPECIFIED.,.F.,.F.,(4,1,2,4),(0.,0.000802008422577636,
0.00160401684514921,0.00313695506663806),.UNSPECIFIED.);
#376=B_SPLINE_CURVE_WITH_KNOTS('',3,(#18665,#18666,#18667,#18668,#18669,
#18670,#18671,#18672,#18673,#18674,#18675,#18676,#18677,#18678,#18679,#18680,
#18681,#18682,#18683,#18684,#18685,#18686,#18687,#18688,#18689,#18690,#18691,
#18692,#18693,#18694,#18695,#18696,#18697,#18698,#18699,#18700,#18701,#18702),
 .UNSPECIFIED.,.F.,.F.,(4,2,2,2,2,2,2,2,2,2,2,2,2,2,2,2,2,2,4),(-0.728274932141156,
-0.62958437370879,-0.513230659588247,-0.435254656595599,-0.382758778659329,
-0.358199460630516,-0.35520801993891,-0.35357862650099,-0.353227607893641,
-0.353002007656128,-0.352824286806013,-0.352623194503785,-0.352288454767916,
-0.351064596075185,-0.343311205277017,-0.312348670606145,-0.254183071767702,
-0.170240832437228,0.),.UNSPECIFIED.);
#377=B_SPLINE_CURVE_WITH_KNOTS('',3,(#18993,#18994,#18995,#18996,#18997,
#18998,#18999),.UNSPECIFIED.,.F.,.F.,(4,1,2,4),(0.,0.000802008422543309,
0.00160401684508538,0.00313356353166786),.UNSPECIFIED.);
#378=B_SPLINE_CURVE_WITH_KNOTS('',3,(#19000,#19001,#19002,#19003,#19004,
#19005),.UNSPECIFIED.,.F.,.F.,(4,2,4),(-0.324384744695224,-0.162317646330996,
0.),.UNSPECIFIED.);
#379=B_SPLINE_CURVE_WITH_KNOTS('',3,(#19298,#19299,#19300,#19301,#19302,
#19303),.UNSPECIFIED.,.F.,.F.,(4,2,4),(-0.222197670544619,-0.111101699996788,
0.),.UNSPECIFIED.);
#380=B_SPLINE_CURVE_WITH_KNOTS('',3,(#19304,#19305,#19306,#19307,#19308,
#19309,#19310,#19311,#19312),.UNSPECIFIED.,.F.,.F.,(4,2,3,4),(0.,0.000802008422904865,
0.00160401684586609,0.00313011409353478),.UNSPECIFIED.);
#381=B_SPLINE_CURVE_WITH_KNOTS('',3,(#19520,#19521,#19522,#19523,#19524,
#19525,#19526,#19527,#19528,#19529,#19530,#19531,#19532,#19533,#19534,#19535,
#19536,#19537,#19538,#19539,#19540,#19541,#19542,#19543,#19544,#19545,#19546,
#19547),.UNSPECIFIED.,.F.,.F.,(4,2,2,2,2,2,2,2,2,2,2,2,2,4),(0.,1.30396391294989,
2.60816609231495,4.56086018974018,6.500232979704,8.45070313715037,10.4269067443957,
12.3773244878899,14.3166724219264,16.2692988357265,18.2429971279301,20.1912804500865,
22.1308341479624,23.6343466236277),.UNSPECIFIED.);
#382=B_SPLINE_CURVE_WITH_KNOTS('',3,(#19553,#19554,#19555,#19556,#19557,
#19558,#19559,#19560,#19561,#19562,#19563,#19564,#19565,#19566,#19567,#19568,
#19569,#19570,#19571,#19572,#19573,#19574,#19575,#19576,#19577,#19578,#19579,
#19580),.UNSPECIFIED.,.F.,.F.,(4,2,2,2,2,2,2,2,2,2,2,2,2,4),(78.502201789525,
80.3928667388685,82.3384972109937,84.2788241322494,86.2377173630452,88.2079834738884,
90.1520350835772,92.0931180658711,94.0544724803042,96.0212222485092,97.9638912741162,
99.9059931283975,101.023430324553,102.135964763307),.UNSPECIFIED.);
#383=B_SPLINE_CURVE_WITH_KNOTS('',3,(#19583,#19584,#19585,#19586,#19587,
#19588,#19589,#19590,#19591,#19592,#19593,#19594,#19595,#19596,#19597,#19598,
#19599,#19600,#19601,#19602,#19603,#19604,#19605,#19606,#19607,#19608,#19609,
#19610,#19611,#19612,#19613,#19614,#19615,#19616,#19617,#19618),
 .UNSPECIFIED.,.F.,.F.,(4,2,2,2,2,2,2,2,2,2,2,2,2,2,2,2,2,4),(23.6343466236277,
24.0859013362698,26.0570400286112,28.003370843106,29.9433774048251,31.9011613014351,
33.869710627465,35.8143050082161,37.7550192764481,39.7157770489108,41.6817334338505,
43.6248336037104,45.5665083217582,47.5304684261993,49.4938551346482,51.435719911611,
53.3785958965145,55.1510718902642),.UNSPECIFIED.);
#384=B_SPLINE_CURVE_WITH_KNOTS('',3,(#19623,#19624,#19625,#19626,#19627,
#19628,#19629,#19630,#19631,#19632,#19633,#19634,#19635,#19636,#19637,#19638,
#19639,#19640,#19641,#19642,#19643,#19644,#19645,#19646,#19647,#19648,#19649,
#19650,#19651,#19652,#19653,#19654,#19655,#19656,#19657,#19658,#19659,#19660),
 .UNSPECIFIED.,.F.,.F.,(4,2,2,2,2,2,2,2,2,2,2,2,2,2,2,2,2,2,4),(46.9842134144311,
47.1683179476468,49.128813348479,51.0696211747879,53.0090557646061,54.9587871273889,
56.9342063154586,58.8854100779273,60.8247947630869,62.7767598037459,64.7546358588809,
66.7038727383019,68.6434231351511,70.5976920946369,72.575259116529,74.5226306638379,
76.4624530680027,78.418977906567,78.502201789525),.UNSPECIFIED.);
#385=B_SPLINE_CURVE_WITH_KNOTS('',3,(#19661,#19662,#19663,#19664,#19665,
#19666,#19667,#19668,#19669,#19670,#19671,#19672,#19673,#19674,#19675,#19676,
#19677,#19678,#19679,#19680,#19681,#19682,#19683,#19684,#19685,#19686,#19687,
#19688,#19689,#19690,#19691,#19692,#19693,#19694,#19695,#19696,#19697,#19698),
 .UNSPECIFIED.,.F.,.F.,(4,2,2,2,2,2,2,2,2,2,2,2,2,2,2,2,2,2,4),(55.1510718902642,
55.3459492191646,57.3068158150841,59.2477103486072,61.1871252191665,63.1364287476564,
65.1113578818397,67.0628817695785,69.0022066891439,70.953719601354,72.9311191528217,
74.8806267146135,76.8200815012103,78.7738929823442,80.7520431717114,82.6996675386312,
84.6393555394773,86.5954010716407,86.6680978070119),.UNSPECIFIED.);
#386=B_SPLINE_CURVE_WITH_KNOTS('',3,(#19704,#19705,#19706,#19707,#19708,
#19709,#19710,#19711,#19712,#19713,#19714,#19715,#19716,#19717,#19718,#19719,
#19720,#19721),.UNSPECIFIED.,.F.,.F.,(4,2,2,2,2,2,2,2,4),(118.184020883807,
118.803694236851,119.279145252132,119.517336391626,119.636434572161,119.695970056689,
119.725732617238,119.740612379807,119.756924319264),.UNSPECIFIED.);
#387=B_SPLINE_CURVE_WITH_KNOTS('',3,(#19726,#19727,#19728,#19729,#19730,
#19731,#19732,#19733,#19734,#19735,#19736,#19737,#19738,#19739,#19740,#19741,
#19742,#19743,#19744,#19745),.UNSPECIFIED.,.F.,.F.,(4,2,2,2,2,2,2,2,2,4),
(9.99999992304919E-7,1.12538984857621,2.24819806101112,4.19829220265297,
6.13771124438825,8.09078865884484,10.0641056167008,12.0120937201665,13.9517598952885,
15.4666452689729),.UNSPECIFIED.);
#388=B_SPLINE_CURVE_WITH_KNOTS('',3,(#19771,#19772,#19773,#19774,#19775,
#19776,#19777,#19778,#19779,#19780,#19781,#19782,#19783,#19784,#19785,#19786,
#19787,#19788,#19789,#19790,#19791,#19792,#19793,#19794,#19795,#19796,#19797,
#19798,#19799,#19800,#19801,#19802,#19803,#19804,#19805,#19806),
 .UNSPECIFIED.,.F.,.F.,(4,2,2,2,2,2,2,2,2,2,2,2,2,2,2,2,2,4),(15.4666452689729,
15.9073263138292,17.8780768344747,19.8241472733818,21.7643097977368,23.7226387447498,
25.690797326506,27.6351711527205,29.576085113709,31.5374294358844,33.5029970868268,
35.4459200800723,37.3878368573986,39.35241917033,41.3154237226985,43.2571565265499,
45.2003139491873,46.9842134144311),.UNSPECIFIED.);
#389=B_SPLINE_CURVE_WITH_KNOTS('',3,(#19807,#19808,#19809,#19810,#19811,
#19812,#19813,#19814,#19815,#19816,#19817,#19818,#19819,#19820,#19821,#19822,
#19823,#19824,#19825,#19826,#19827,#19828,#19829,#19830,#19831,#19832,#19833,
#19834,#19835,#19836,#19837,#19838,#19839,#19840,#19841,#19842),
 .UNSPECIFIED.,.F.,.F.,(4,2,2,2,2,2,2,2,2,2,2,2,2,2,2,2,2,4),(86.6680978070119,
88.5698686964051,90.5157271678372,92.4558768432157,94.4142720649564,96.3851035202131,
98.329351784228,100.27021180681,102.231053249456,104.198345974643,106.141174650795,
108.083006466375,110.046368338904,112.010268920263,113.951897726735,115.894966472163,
117.860898185085,118.184020883807),.UNSPECIFIED.);
#390=B_SPLINE_CURVE_WITH_KNOTS('',3,(#20083,#20084,#20085,#20086,#20087,
#20088,#20089,#20090,#20091,#20092,#20093,#20094,#20095,#20096,#20097,#20098,
#20099,#20100),.UNSPECIFIED.,.F.,.F.,(4,2,2,2,2,2,2,2,4),(0.,0.978481252991969,
1.98438926043037,3.83556386007751,4.8022813892872,5.7579599217032,7.83058544513618,
8.89308643237631,9.98441482005272),.UNSPECIFIED.);
#391=B_SPLINE_CURVE_WITH_KNOTS('',3,(#20526,#20527,#20528,#20529,#20530,
#20531,#20532,#20533,#20534,#20535,#20536,#20537,#20538,#20539,#20540,#20541,
#20542,#20543,#20544,#20545,#20546,#20547),.UNSPECIFIED.,.F.,.F.,(4,2,2,
2,2,2,2,2,2,2,4),(1.27322512801248,1.33474273520392,1.47506259652504,1.63354487754016,
1.7891729428134,1.93308978701607,2.07370553081328,2.22765816465705,2.39186406247873,
2.46887047840366,2.54509076244393),.UNSPECIFIED.);
#392=B_SPLINE_CURVE_WITH_KNOTS('',3,(#20567,#20568,#20569,#20570,#20571,
#20572,#20573,#20574,#20575,#20576,#20577,#20578,#20579,#20580,#20581,#20582,
#20583,#20584,#20585,#20586),.UNSPECIFIED.,.F.,.F.,(4,2,2,2,2,2,2,2,2,4),
(0.,0.133781719517655,0.281821942641468,0.447759981880601,0.597114390464313,
0.737248938214622,0.881128826876862,1.04037144466368,1.19403526065854,1.27322512801215),
 .UNSPECIFIED.);
#393=PLANE('',#3805);
#394=PLANE('',#3806);
#395=PLANE('',#3811);
#396=PLANE('',#3812);
#397=PLANE('',#3892);
#398=PLANE('',#3894);
#399=PLANE('',#3896);
#400=PLANE('',#3897);
#401=PLANE('',#3917);
#402=PLANE('',#3918);
#403=PLANE('',#3919);
#404=PLANE('',#3920);
#405=PLANE('',#3922);
#406=PLANE('',#3923);
#407=PLANE('',#3924);
#408=PLANE('',#3925);
#409=PLANE('',#3926);
#410=PLANE('',#3927);
#411=PLANE('',#3928);
#412=PLANE('',#3929);
#413=PLANE('',#3930);
#414=PLANE('',#3931);
#415=PLANE('',#3958);
#416=PLANE('',#3960);
#417=PLANE('',#3961);
#418=PLANE('',#3962);
#419=PLANE('',#3963);
#420=PLANE('',#3964);
#421=PLANE('',#3965);
#422=PLANE('',#3970);
#423=PLANE('',#3971);
#424=PLANE('',#3979);
#425=PLANE('',#3980);
#426=PLANE('',#3988);
#427=PLANE('',#3989);
#428=PLANE('',#4012);
#429=PLANE('',#4013);
#430=PLANE('',#4014);
#431=PLANE('',#4016);
#432=PLANE('',#4017);
#433=PLANE('',#4018);
#434=PLANE('',#4019);
#435=PLANE('',#4020);
#436=PLANE('',#4021);
#437=PLANE('',#4070);
#438=PLANE('',#4071);
#439=PLANE('',#4091);
#440=PLANE('',#4093);
#441=PLANE('',#4095);
#442=PLANE('',#4096);
#443=PLANE('',#4097);
#444=PLANE('',#4098);
#445=PLANE('',#4099);
#446=PLANE('',#4100);
#447=PLANE('',#4102);
#448=LINE('',#4999,#641);
#449=LINE('',#5008,#642);
#450=LINE('',#5017,#643);
#451=LINE('',#5023,#644);
#452=LINE('',#5047,#645);
#453=LINE('',#5097,#646);
#454=LINE('',#5120,#647);
#455=LINE('',#5124,#648);
#456=LINE('',#5145,#649);
#457=LINE('',#5149,#650);
#458=LINE('',#5164,#651);
#459=LINE('',#5178,#652);
#460=LINE('',#5182,#653);
#461=LINE('',#5203,#654);
#462=LINE('',#5206,#655);
#463=LINE('',#5210,#656);
#464=LINE('',#5220,#657);
#465=LINE('',#5231,#658);
#466=LINE('',#5255,#659);
#467=LINE('',#5265,#660);
#468=LINE('',#5276,#661);
#469=LINE('',#5286,#662);
#470=LINE('',#5297,#663);
#471=LINE('',#5307,#664);
#472=LINE('',#5318,#665);
#473=LINE('',#5328,#666);
#474=LINE('',#5339,#667);
#475=LINE('',#5349,#668);
#476=LINE('',#5360,#669);
#477=LINE('',#5370,#670);
#478=LINE('',#5381,#671);
#479=LINE('',#5391,#672);
#480=LINE('',#5402,#673);
#481=LINE('',#5412,#674);
#482=LINE('',#5417,#675);
#483=LINE('',#5427,#676);
#484=LINE('',#5438,#677);
#485=LINE('',#5448,#678);
#486=LINE('',#5459,#679);
#487=LINE('',#5469,#680);
#488=LINE('',#5480,#681);
#489=LINE('',#5490,#682);
#490=LINE('',#5501,#683);
#491=LINE('',#5511,#684);
#492=LINE('',#5522,#685);
#493=LINE('',#5532,#686);
#494=LINE('',#8030,#687);
#495=LINE('',#8334,#688);
#496=LINE('',#10866,#689);
#497=LINE('',#10867,#690);
#498=LINE('',#10870,#691);
#499=LINE('',#10879,#692);
#500=LINE('',#10890,#693);
#501=LINE('',#10891,#694);
#502=LINE('',#10894,#695);
#503=LINE('',#10903,#696);
#504=LINE('',#10914,#697);
#505=LINE('',#10915,#698);
#506=LINE('',#10918,#699);
#507=LINE('',#10927,#700);
#508=LINE('',#10938,#701);
#509=LINE('',#10939,#702);
#510=LINE('',#10942,#703);
#511=LINE('',#10951,#704);
#512=LINE('',#10954,#705);
#513=LINE('',#10963,#706);
#514=LINE('',#10966,#707);
#515=LINE('',#10975,#708);
#516=LINE('',#10986,#709);
#517=LINE('',#10987,#710);
#518=LINE('',#10990,#711);
#519=LINE('',#10999,#712);
#520=LINE('',#11010,#713);
#521=LINE('',#11011,#714);
#522=LINE('',#11014,#715);
#523=LINE('',#11023,#716);
#524=LINE('',#11034,#717);
#525=LINE('',#11035,#718);
#526=LINE('',#11038,#719);
#527=LINE('',#11048,#720);
#528=LINE('',#11063,#721);
#529=LINE('',#11064,#722);
#530=LINE('',#11076,#723);
#531=LINE('',#11090,#724);
#532=LINE('',#11102,#725);
#533=LINE('',#11428,#726);
#534=LINE('',#13877,#727);
#535=LINE('',#13886,#728);
#536=LINE('',#16883,#729);
#537=LINE('',#16886,#730);
#538=LINE('',#16888,#731);
#539=LINE('',#16891,#732);
#540=LINE('',#16893,#733);
#541=LINE('',#16895,#734);
#542=LINE('',#16898,#735);
#543=LINE('',#16899,#736);
#544=LINE('',#16901,#737);
#545=LINE('',#16902,#738);
#546=LINE('',#16906,#739);
#547=LINE('',#16922,#740);
#548=LINE('',#16939,#741);
#549=LINE('',#16974,#742);
#550=LINE('',#16998,#743);
#551=LINE('',#17959,#744);
#552=LINE('',#18272,#745);
#553=LINE('',#18317,#746);
#554=LINE('',#18340,#747);
#555=LINE('',#18341,#748);
#556=LINE('',#18344,#749);
#557=LINE('',#19297,#750);
#558=LINE('',#19314,#751);
#559=LINE('',#19315,#752);
#560=LINE('',#19316,#753);
#561=LINE('',#19317,#754);
#562=LINE('',#19319,#755);
#563=LINE('',#19320,#756);
#564=LINE('',#19323,#757);
#565=LINE('',#19324,#758);
#566=LINE('',#19326,#759);
#567=LINE('',#19328,#760);
#568=LINE('',#19330,#761);
#569=LINE('',#19331,#762);
#570=LINE('',#19339,#763);
#571=LINE('',#19340,#764);
#572=LINE('',#19355,#765);
#573=LINE('',#19363,#766);
#574=LINE('',#19376,#767);
#575=LINE('',#19430,#768);
#576=LINE('',#19484,#769);
#577=LINE('',#19500,#770);
#578=LINE('',#19517,#771);
#579=LINE('',#19551,#772);
#580=LINE('',#19581,#773);
#581=LINE('',#19622,#774);
#582=LINE('',#19702,#775);
#583=LINE('',#19723,#776);
#584=LINE('',#19750,#777);
#585=LINE('',#19756,#778);
#586=LINE('',#19762,#779);
#587=LINE('',#19768,#780);
#588=LINE('',#19844,#781);
#589=LINE('',#19845,#782);
#590=LINE('',#20101,#783);
#591=LINE('',#20105,#784);
#592=LINE('',#20304,#785);
#593=LINE('',#20313,#786);
#594=LINE('',#20319,#787);
#595=LINE('',#20328,#788);
#596=LINE('',#20334,#789);
#597=LINE('',#20343,#790);
#598=LINE('',#20349,#791);
#599=LINE('',#20355,#792);
#600=LINE('',#20361,#793);
#601=LINE('',#20367,#794);
#602=LINE('',#20373,#795);
#603=LINE('',#20379,#796);
#604=LINE('',#20388,#797);
#605=LINE('',#20390,#798);
#606=LINE('',#20392,#799);
#607=LINE('',#20393,#800);
#608=LINE('',#20397,#801);
#609=LINE('',#20399,#802);
#610=LINE('',#20401,#803);
#611=LINE('',#20402,#804);
#612=LINE('',#20406,#805);
#613=LINE('',#20408,#806);
#614=LINE('',#20410,#807);
#615=LINE('',#20411,#808);
#616=LINE('',#20415,#809);
#617=LINE('',#20417,#810);
#618=LINE('',#20419,#811);
#619=LINE('',#20420,#812);
#620=LINE('',#20424,#813);
#621=LINE('',#20426,#814);
#622=LINE('',#20428,#815);
#623=LINE('',#20429,#816);
#624=LINE('',#20433,#817);
#625=LINE('',#20435,#818);
#626=LINE('',#20437,#819);
#627=LINE('',#20438,#820);
#628=LINE('',#20488,#821);
#629=LINE('',#20510,#822);
#630=LINE('',#20514,#823);
#631=LINE('',#20519,#824);
#632=LINE('',#20551,#825);
#633=LINE('',#20557,#826);
#634=LINE('',#20561,#827);
#635=LINE('',#20592,#828);
#636=LINE('',#20593,#829);
#637=LINE('',#20595,#830);
#638=LINE('',#20596,#831);
#639=LINE('',#20598,#832);
#640=LINE('',#20600,#833);
#641=VECTOR('',#4145,3.96875);
#642=VECTOR('',#4158,3.96875);
#643=VECTOR('',#4171,40.);
#644=VECTOR('',#4178,46.);
#645=VECTOR('',#4187,40.);
#646=VECTOR('',#4198,1000.);
#647=VECTOR('',#4201,1000.);
#648=VECTOR('',#4204,1000.);
#649=VECTOR('',#4205,1000.);
#650=VECTOR('',#4208,10.);
#651=VECTOR('',#4209,36.);
#652=VECTOR('',#4212,1000.);
#653=VECTOR('',#4215,1000.);
#654=VECTOR('',#4216,1000.);
#655=VECTOR('',#4219,1000.);
#656=VECTOR('',#4222,1000.);
#657=VECTOR('',#4223,1000.);
#658=VECTOR('',#4226,1000.);
#659=VECTOR('',#4229,1000.);
#660=VECTOR('',#4230,1000.);
#661=VECTOR('',#4233,1000.);
#662=VECTOR('',#4234,1000.);
#663=VECTOR('',#4237,1000.);
#664=VECTOR('',#4238,1000.);
#665=VECTOR('',#4241,1000.);
#666=VECTOR('',#4242,1000.);
#667=VECTOR('',#4245,1000.);
#668=VECTOR('',#4246,1000.);
#669=VECTOR('',#4249,1000.);
#670=VECTOR('',#4250,1000.);
#671=VECTOR('',#4253,1000.);
#672=VECTOR('',#4254,1000.);
#673=VECTOR('',#4257,1000.);
#674=VECTOR('',#4258,1000.);
#675=VECTOR('',#4263,1000.);
#676=VECTOR('',#4264,1000.);
#677=VECTOR('',#4267,1000.);
#678=VECTOR('',#4268,1000.);
#679=VECTOR('',#4271,1000.);
#680=VECTOR('',#4272,1000.);
#681=VECTOR('',#4275,1000.);
#682=VECTOR('',#4276,1000.);
#683=VECTOR('',#4279,1000.);
#684=VECTOR('',#4280,1000.);
#685=VECTOR('',#4283,1000.);
#686=VECTOR('',#4284,1000.);
#687=VECTOR('',#4293,10.);
#688=VECTOR('',#4298,10.);
#689=VECTOR('',#4311,10.);
#690=VECTOR('',#4312,10.);
#691=VECTOR('',#4315,10.);
#692=VECTOR('',#4316,10.);
#693=VECTOR('',#4319,10.);
#694=VECTOR('',#4320,10.);
#695=VECTOR('',#4323,10.);
#696=VECTOR('',#4324,10.);
#697=VECTOR('',#4327,10.);
#698=VECTOR('',#4328,10.);
#699=VECTOR('',#4331,10.);
#700=VECTOR('',#4332,10.);
#701=VECTOR('',#4335,10.);
#702=VECTOR('',#4336,10.);
#703=VECTOR('',#4339,10.);
#704=VECTOR('',#4340,10.);
#705=VECTOR('',#4343,10.);
#706=VECTOR('',#4344,10.);
#707=VECTOR('',#4347,10.);
#708=VECTOR('',#4348,10.);
#709=VECTOR('',#4351,10.);
#710=VECTOR('',#4352,10.);
#711=VECTOR('',#4355,10.);
#712=VECTOR('',#4356,10.);
#713=VECTOR('',#4359,10.);
#714=VECTOR('',#4360,10.);
#715=VECTOR('',#4363,10.);
#716=VECTOR('',#4364,10.);
#717=VECTOR('',#4367,10.);
#718=VECTOR('',#4368,10.);
#719=VECTOR('',#4371,10.);
#720=VECTOR('',#4372,10.);
#721=VECTOR('',#4375,10.);
#722=VECTOR('',#4376,10.);
#723=VECTOR('',#4379,10.);
#724=VECTOR('',#4380,10.);
#725=VECTOR('',#4383,10.);
#726=VECTOR('',#4384,10.);
#727=VECTOR('',#4387,10.);
#728=VECTOR('',#4388,10.);
#729=VECTOR('',#4407,1000.);
#730=VECTOR('',#4410,1000.);
#731=VECTOR('',#4413,1000.);
#732=VECTOR('',#4416,1000.);
#733=VECTOR('',#4419,1000.);
#734=VECTOR('',#4420,1000.);
#735=VECTOR('',#4425,1000.);
#736=VECTOR('',#4426,1000.);
#737=VECTOR('',#4429,1000.);
#738=VECTOR('',#4430,1000.);
#739=VECTOR('',#4433,1000.);
#740=VECTOR('',#4434,1000.);
#741=VECTOR('',#4437,1000.);
#742=VECTOR('',#4440,1000.);
#743=VECTOR('',#4443,1000.);
#744=VECTOR('',#4446,10.);
#745=VECTOR('',#4447,10.);
#746=VECTOR('',#4452,10.);
#747=VECTOR('',#4455,10.);
#748=VECTOR('',#4456,10.);
#749=VECTOR('',#4459,10.);
#750=VECTOR('',#4464,10.);
#751=VECTOR('',#4467,1000.);
#752=VECTOR('',#4468,1000.);
#753=VECTOR('',#4469,1000.);
#754=VECTOR('',#4470,1000.);
#755=VECTOR('',#4473,1000.);
#756=VECTOR('',#4474,1000.);
#757=VECTOR('',#4477,1000.);
#758=VECTOR('',#4478,1000.);
#759=VECTOR('',#4481,1000.);
#760=VECTOR('',#4484,1000.);
#761=VECTOR('',#4487,1000.);
#762=VECTOR('',#4488,1000.);
#763=VECTOR('',#4503,1000.);
#764=VECTOR('',#4504,1000.);
#765=VECTOR('',#4529,47.293670625);
#766=VECTOR('',#4532,10.);
#767=VECTOR('',#4535,47.293670625);
#768=VECTOR('',#4538,47.293670625);
#769=VECTOR('',#4541,47.293670625);
#770=VECTOR('',#4542,10.);
#771=VECTOR('',#4545,50.);
#772=VECTOR('',#4550,50.);
#773=VECTOR('',#4551,1000.);
#774=VECTOR('',#4556,50.);
#775=VECTOR('',#4559,50.);
#776=VECTOR('',#4560,1000.);
#777=VECTOR('',#4567,52.5);
#778=VECTOR('',#4574,52.5);
#779=VECTOR('',#4581,56.);
#780=VECTOR('',#4588,50.);
#781=VECTOR('',#4595,1000.);
#782=VECTOR('',#4596,10.);
#783=VECTOR('',#4599,10.);
#784=VECTOR('',#4606,10.);
#785=VECTOR('',#4619,52.5);
#786=VECTOR('',#4632,16.7);
#787=VECTOR('',#4639,40.);
#788=VECTOR('',#4652,14.8);
#789=VECTOR('',#4659,16.7);
#790=VECTOR('',#4672,13.5);
#791=VECTOR('',#4679,16.7);
#792=VECTOR('',#4686,5.);
#793=VECTOR('',#4693,5.);
#794=VECTOR('',#4700,5.);
#795=VECTOR('',#4707,5.);
#796=VECTOR('',#4714,50.);
#797=VECTOR('',#4727,1000.);
#798=VECTOR('',#4728,1000.);
#799=VECTOR('',#4729,1000.);
#800=VECTOR('',#4730,1000.);
#801=VECTOR('',#4733,1000.);
#802=VECTOR('',#4734,1000.);
#803=VECTOR('',#4735,1000.);
#804=VECTOR('',#4736,1000.);
#805=VECTOR('',#4739,1000.);
#806=VECTOR('',#4740,1000.);
#807=VECTOR('',#4741,1000.);
#808=VECTOR('',#4742,1000.);
#809=VECTOR('',#4745,1000.);
#810=VECTOR('',#4746,1000.);
#811=VECTOR('',#4747,1000.);
#812=VECTOR('',#4748,1000.);
#813=VECTOR('',#4751,1000.);
#814=VECTOR('',#4752,1000.);
#815=VECTOR('',#4753,1000.);
#816=VECTOR('',#4754,1000.);
#817=VECTOR('',#4757,1000.);
#818=VECTOR('',#4758,1000.);
#819=VECTOR('',#4759,1000.);
#820=VECTOR('',#4760,1000.);
#821=VECTOR('',#4855,3.96875);
#822=VECTOR('',#4874,6.35000000000001);
#823=VECTOR('',#4877,1000.);
#824=VECTOR('',#4882,1000.);
#825=VECTOR('',#4891,7.93750000000001);
#826=VECTOR('',#4896,1000.);
#827=VECTOR('',#4899,1000.);
#828=VECTOR('',#4916,1000.);
#829=VECTOR('',#4917,1000.);
#830=VECTOR('',#4920,1000.);
#831=VECTOR('',#4921,1000.);
#832=VECTOR('',#4924,1000.);
#833=VECTOR('',#4927,1000.);
#834=CYLINDRICAL_SURFACE('',#3802,3.96875);
#835=CYLINDRICAL_SURFACE('',#3808,3.96875);
#836=CYLINDRICAL_SURFACE('',#3814,40.);
#837=CYLINDRICAL_SURFACE('',#3817,46.);
#838=CYLINDRICAL_SURFACE('',#3820,40.);
#839=CYLINDRICAL_SURFACE('',#3825,46.);
#840=CYLINDRICAL_SURFACE('',#3828,36.);
#841=CYLINDRICAL_SURFACE('',#3834,46.);
#842=CYLINDRICAL_SURFACE('',#3835,46.);
#843=CYLINDRICAL_SURFACE('',#3836,46.);
#844=CYLINDRICAL_SURFACE('',#3837,46.);
#845=CYLINDRICAL_SURFACE('',#3838,46.);
#846=CYLINDRICAL_SURFACE('',#3839,46.);
#847=CYLINDRICAL_SURFACE('',#3840,46.);
#848=CYLINDRICAL_SURFACE('',#3841,46.);
#849=CYLINDRICAL_SURFACE('',#3842,46.);
#850=CYLINDRICAL_SURFACE('',#3843,46.);
#851=CYLINDRICAL_SURFACE('',#3845,46.);
#852=CYLINDRICAL_SURFACE('',#3846,46.);
#853=CYLINDRICAL_SURFACE('',#3847,46.);
#854=CYLINDRICAL_SURFACE('',#3848,46.);
#855=CYLINDRICAL_SURFACE('',#3849,46.);
#856=CYLINDRICAL_SURFACE('',#3850,46.);
#857=CYLINDRICAL_SURFACE('',#3862,48.7063293749999);
#858=CYLINDRICAL_SURFACE('',#3863,48.7063293749999);
#859=CYLINDRICAL_SURFACE('',#3864,48.7063293749999);
#860=CYLINDRICAL_SURFACE('',#3865,48.7063293749999);
#861=CYLINDRICAL_SURFACE('',#3866,48.7063293749999);
#862=CYLINDRICAL_SURFACE('',#3867,48.7063293749999);
#863=CYLINDRICAL_SURFACE('',#3868,48.7063293749999);
#864=CYLINDRICAL_SURFACE('',#3869,48.7063293749999);
#865=CYLINDRICAL_SURFACE('',#3870,48.7063293749999);
#866=CYLINDRICAL_SURFACE('',#3871,48.7063293749999);
#867=CYLINDRICAL_SURFACE('',#3872,48.7063293749999);
#868=CYLINDRICAL_SURFACE('',#3873,48.7063293749999);
#869=CYLINDRICAL_SURFACE('',#3874,48.7063293749999);
#870=CYLINDRICAL_SURFACE('',#3875,48.7063293749999);
#871=CYLINDRICAL_SURFACE('',#3876,48.7063293749999);
#872=CYLINDRICAL_SURFACE('',#3877,48.7063293749999);
#873=CYLINDRICAL_SURFACE('',#3878,48.7063293749999);
#874=CYLINDRICAL_SURFACE('',#3879,48.7063293749999);
#875=CYLINDRICAL_SURFACE('',#3880,48.7063293749999);
#876=CYLINDRICAL_SURFACE('',#3890,48.5805105169702);
#877=CYLINDRICAL_SURFACE('',#3898,46.);
#878=CYLINDRICAL_SURFACE('',#3899,46.);
#879=CYLINDRICAL_SURFACE('',#3900,46.);
#880=CYLINDRICAL_SURFACE('',#3901,46.);
#881=CYLINDRICAL_SURFACE('',#3904,48.7063293749999);
#882=CYLINDRICAL_SURFACE('',#3905,48.7063293749999);
#883=CYLINDRICAL_SURFACE('',#3906,48.7063293749999);
#884=CYLINDRICAL_SURFACE('',#3909,3.96875);
#885=CYLINDRICAL_SURFACE('',#3910,3.96875);
#886=CYLINDRICAL_SURFACE('',#3912,46.);
#887=CYLINDRICAL_SURFACE('',#3913,48.5805105169702);
#888=CYLINDRICAL_SURFACE('',#3914,3.96875);
#889=CYLINDRICAL_SURFACE('',#3915,46.);
#890=CYLINDRICAL_SURFACE('',#3921,3.96875);
#891=CYLINDRICAL_SURFACE('',#3933,47.293670625);
#892=CYLINDRICAL_SURFACE('',#3935,47.293670625);
#893=CYLINDRICAL_SURFACE('',#3936,47.293670625);
#894=CYLINDRICAL_SURFACE('',#3937,47.293670625);
#895=CYLINDRICAL_SURFACE('',#3938,50.);
#896=CYLINDRICAL_SURFACE('',#3940,50.);
#897=CYLINDRICAL_SURFACE('',#3942,50.);
#898=CYLINDRICAL_SURFACE('',#3943,50.);
#899=CYLINDRICAL_SURFACE('',#3945,52.5);
#900=CYLINDRICAL_SURFACE('',#3948,52.5);
#901=CYLINDRICAL_SURFACE('',#3951,56.);
#902=CYLINDRICAL_SURFACE('',#3954,50.);
#903=CYLINDRICAL_SURFACE('',#3957,50.);
#904=CYLINDRICAL_SURFACE('',#3959,47.293670625);
#905=CYLINDRICAL_SURFACE('',#3967,52.5);
#906=CYLINDRICAL_SURFACE('',#3973,16.7);
#907=CYLINDRICAL_SURFACE('',#3976,40.);
#908=CYLINDRICAL_SURFACE('',#3982,14.8);
#909=CYLINDRICAL_SURFACE('',#3985,16.7);
#910=CYLINDRICAL_SURFACE('',#3991,13.5);
#911=CYLINDRICAL_SURFACE('',#3994,16.7);
#912=CYLINDRICAL_SURFACE('',#3997,5.);
#913=CYLINDRICAL_SURFACE('',#4000,5.);
#914=CYLINDRICAL_SURFACE('',#4003,5.);
#915=CYLINDRICAL_SURFACE('',#4006,5.);
#916=CYLINDRICAL_SURFACE('',#4009,50.);
#917=CYLINDRICAL_SURFACE('',#4022,1.);
#918=CYLINDRICAL_SURFACE('',#4031,1.);
#919=CYLINDRICAL_SURFACE('',#4033,1.);
#920=CYLINDRICAL_SURFACE('',#4035,1.);
#921=CYLINDRICAL_SURFACE('',#4038,1.);
#922=CYLINDRICAL_SURFACE('',#4040,1.);
#923=CYLINDRICAL_SURFACE('',#4042,1.);
#924=CYLINDRICAL_SURFACE('',#4053,1.);
#925=CYLINDRICAL_SURFACE('',#4055,1.);
#926=CYLINDRICAL_SURFACE('',#4057,1.);
#927=CYLINDRICAL_SURFACE('',#4059,1.);
#928=CYLINDRICAL_SURFACE('',#4065,1.);
#929=CYLINDRICAL_SURFACE('',#4067,3.96875);
#930=CYLINDRICAL_SURFACE('',#4076,6.35000000000001);
#931=CYLINDRICAL_SURFACE('',#4082,7.93750000000001);
#932=SHAPE_REPRESENTATION_RELATIONSHIP('SRR','None',#20716,#944);
#933=SHAPE_REPRESENTATION_RELATIONSHIP('SRR','None',#20717,#945);
#934=SHAPE_REPRESENTATION_RELATIONSHIP('SRR','None',#20718,#946);
#935=SHAPE_REPRESENTATION_RELATIONSHIP('SRR','None',#20719,#947);
#936=SHAPE_REPRESENTATION_RELATIONSHIP('SRR','None',#20720,#948);
#937=SHAPE_REPRESENTATION_RELATIONSHIP('SRR','None',#20721,#949);
#938=SHAPE_REPRESENTATION_RELATIONSHIP('SRR','None',#20722,#950);
#939=SHAPE_REPRESENTATION_RELATIONSHIP('SRR','None',#20723,#951);
#940=SHAPE_REPRESENTATION_RELATIONSHIP('SRR','None',#20724,#952);
#941=SHAPE_REPRESENTATION_RELATIONSHIP('SRR','None',#20725,#953);
#942=SHAPE_REPRESENTATION_RELATIONSHIP('SRR','None',#20726,#954);
#943=SHAPE_REPRESENTATION_RELATIONSHIP('SRR','None',#20727,#955);
#944=ADVANCED_BREP_SHAPE_REPRESENTATION('',(#968),#20646);
#945=ADVANCED_BREP_SHAPE_REPRESENTATION('',(#969),#20647);
#946=ADVANCED_BREP_SHAPE_REPRESENTATION('',(#970),#20648);
#947=ADVANCED_BREP_SHAPE_REPRESENTATION('',(#971),#20649);
#948=ADVANCED_BREP_SHAPE_REPRESENTATION('',(#972),#20650);
#949=ADVANCED_BREP_SHAPE_REPRESENTATION('',(#973),#20651);
#950=ADVANCED_BREP_SHAPE_REPRESENTATION('',(#974),#20652);
#951=ADVANCED_BREP_SHAPE_REPRESENTATION('',(#975),#20653);
#952=ADVANCED_BREP_SHAPE_REPRESENTATION('',(#976),#20654);
#953=ADVANCED_BREP_SHAPE_REPRESENTATION('',(#977),#20655);
#954=ADVANCED_BREP_SHAPE_REPRESENTATION('',(#978),#20656);
#955=ADVANCED_BREP_SHAPE_REPRESENTATION('',(#979),#20657);
#956=STYLED_ITEM('',(#20785),#968);
#957=STYLED_ITEM('',(#20785),#969);
#958=STYLED_ITEM('',(#20785),#970);
#959=STYLED_ITEM('',(#20786),#971);
#960=STYLED_ITEM('',(#20787),#972);
#961=STYLED_ITEM('',(#20786),#973);
#962=STYLED_ITEM('',(#20785),#974);
#963=STYLED_ITEM('',(#20787),#975);
#964=STYLED_ITEM('',(#20788),#976);
#965=STYLED_ITEM('',(#20786),#977);
#966=STYLED_ITEM('',(#20786),#978);
#967=STYLED_ITEM('',(#20786),#979);
#968=MANIFOLD_SOLID_BREP('Body1',#3651);
#969=MANIFOLD_SOLID_BREP('Body1',#3652);
#970=MANIFOLD_SOLID_BREP('Body1',#3653);
#971=MANIFOLD_SOLID_BREP('Body1',#3654);
#972=MANIFOLD_SOLID_BREP('Body1',#3655);
#973=MANIFOLD_SOLID_BREP('Body1',#3656);
#974=MANIFOLD_SOLID_BREP('Body1',#3657);
#975=MANIFOLD_SOLID_BREP('Body1',#3658);
#976=MANIFOLD_SOLID_BREP('Body1',#3659);
#977=MANIFOLD_SOLID_BREP('Body1',#3660);
#978=MANIFOLD_SOLID_BREP('Body1',#3661);
#979=MANIFOLD_SOLID_BREP('Body1',#3662);
#980=FACE_OUTER_BOUND('',#1189,.T.);
#981=FACE_OUTER_BOUND('',#1190,.T.);
#982=FACE_OUTER_BOUND('',#1191,.T.);
#983=FACE_OUTER_BOUND('',#1192,.T.);
#984=FACE_OUTER_BOUND('',#1193,.T.);
#985=FACE_OUTER_BOUND('',#1194,.T.);
#986=FACE_OUTER_BOUND('',#1195,.T.);
#987=FACE_OUTER_BOUND('',#1196,.T.);
#988=FACE_OUTER_BOUND('',#1197,.T.);
#989=FACE_OUTER_BOUND('',#1198,.T.);
#990=FACE_OUTER_BOUND('',#1199,.T.);
#991=FACE_OUTER_BOUND('',#1200,.T.);
#992=FACE_OUTER_BOUND('',#1201,.T.);
#993=FACE_OUTER_BOUND('',#1202,.T.);
#994=FACE_OUTER_BOUND('',#1203,.T.);
#995=FACE_OUTER_BOUND('',#1204,.T.);
#996=FACE_OUTER_BOUND('',#1205,.T.);
#997=FACE_OUTER_BOUND('',#1206,.T.);
#998=FACE_OUTER_BOUND('',#1207,.T.);
#999=FACE_OUTER_BOUND('',#1208,.T.);
#1000=FACE_OUTER_BOUND('',#1209,.T.);
#1001=FACE_OUTER_BOUND('',#1210,.T.);
#1002=FACE_OUTER_BOUND('',#1211,.T.);
#1003=FACE_OUTER_BOUND('',#1212,.T.);
#1004=FACE_OUTER_BOUND('',#1213,.T.);
#1005=FACE_OUTER_BOUND('',#1214,.T.);
#1006=FACE_OUTER_BOUND('',#1215,.T.);
#1007=FACE_OUTER_BOUND('',#1216,.T.);
#1008=FACE_OUTER_BOUND('',#1217,.T.);
#1009=FACE_OUTER_BOUND('',#1218,.T.);
#1010=FACE_OUTER_BOUND('',#1219,.T.);
#1011=FACE_OUTER_BOUND('',#1220,.T.);
#1012=FACE_OUTER_BOUND('',#1221,.T.);
#1013=FACE_OUTER_BOUND('',#1222,.T.);
#1014=FACE_OUTER_BOUND('',#1223,.T.);
#1015=FACE_OUTER_BOUND('',#1224,.T.);
#1016=FACE_OUTER_BOUND('',#1225,.T.);
#1017=FACE_OUTER_BOUND('',#1226,.T.);
#1018=FACE_OUTER_BOUND('',#1227,.T.);
#1019=FACE_OUTER_BOUND('',#1228,.T.);
#1020=FACE_OUTER_BOUND('',#1229,.T.);
#1021=FACE_OUTER_BOUND('',#1230,.T.);
#1022=FACE_OUTER_BOUND('',#1231,.T.);
#1023=FACE_OUTER_BOUND('',#1232,.T.);
#1024=FACE_OUTER_BOUND('',#1233,.T.);
#1025=FACE_OUTER_BOUND('',#1234,.T.);
#1026=FACE_OUTER_BOUND('',#1235,.T.);
#1027=FACE_OUTER_BOUND('',#1236,.T.);
#1028=FACE_OUTER_BOUND('',#1237,.T.);
#1029=FACE_OUTER_BOUND('',#1238,.T.);
#1030=FACE_OUTER_BOUND('',#1239,.T.);
#1031=FACE_OUTER_BOUND('',#1240,.T.);
#1032=FACE_OUTER_BOUND('',#1241,.T.);
#1033=FACE_OUTER_BOUND('',#1242,.T.);
#1034=FACE_OUTER_BOUND('',#1243,.T.);
#1035=FACE_OUTER_BOUND('',#1244,.T.);
#1036=FACE_OUTER_BOUND('',#1245,.T.);
#1037=FACE_OUTER_BOUND('',#1246,.T.);
#1038=FACE_OUTER_BOUND('',#1247,.T.);
#1039=FACE_OUTER_BOUND('',#1248,.T.);
#1040=FACE_OUTER_BOUND('',#1249,.T.);
#1041=FACE_OUTER_BOUND('',#1250,.T.);
#1042=FACE_OUTER_BOUND('',#1251,.T.);
#1043=FACE_OUTER_BOUND('',#1252,.T.);
#1044=FACE_OUTER_BOUND('',#1253,.T.);
#1045=FACE_OUTER_BOUND('',#1254,.T.);
#1046=FACE_OUTER_BOUND('',#1255,.T.);
#1047=FACE_OUTER_BOUND('',#1256,.T.);
#1048=FACE_OUTER_BOUND('',#1257,.T.);
#1049=FACE_OUTER_BOUND('',#1258,.T.);
#1050=FACE_OUTER_BOUND('',#1259,.T.);
#1051=FACE_OUTER_BOUND('',#1260,.T.);
#1052=FACE_OUTER_BOUND('',#1261,.T.);
#1053=FACE_OUTER_BOUND('',#1262,.T.);
#1054=FACE_OUTER_BOUND('',#1263,.T.);
#1055=FACE_OUTER_BOUND('',#1264,.T.);
#1056=FACE_OUTER_BOUND('',#1265,.T.);
#1057=FACE_OUTER_BOUND('',#1266,.T.);
#1058=FACE_OUTER_BOUND('',#1267,.T.);
#1059=FACE_OUTER_BOUND('',#1268,.T.);
#1060=FACE_OUTER_BOUND('',#1269,.T.);
#1061=FACE_OUTER_BOUND('',#1270,.T.);
#1062=FACE_OUTER_BOUND('',#1271,.T.);
#1063=FACE_OUTER_BOUND('',#1272,.T.);
#1064=FACE_OUTER_BOUND('',#1273,.T.);
#1065=FACE_OUTER_BOUND('',#1274,.T.);
#1066=FACE_OUTER_BOUND('',#1275,.T.);
#1067=FACE_OUTER_BOUND('',#1276,.T.);
#1068=FACE_OUTER_BOUND('',#1277,.T.);
#1069=FACE_OUTER_BOUND('',#1278,.T.);
#1070=FACE_OUTER_BOUND('',#1279,.T.);
#1071=FACE_OUTER_BOUND('',#1280,.T.);
#1072=FACE_OUTER_BOUND('',#1281,.T.);
#1073=FACE_OUTER_BOUND('',#1282,.T.);
#1074=FACE_OUTER_BOUND('',#1283,.T.);
#1075=FACE_OUTER_BOUND('',#1284,.T.);
#1076=FACE_OUTER_BOUND('',#1285,.T.);
#1077=FACE_OUTER_BOUND('',#1286,.T.);
#1078=FACE_OUTER_BOUND('',#1287,.T.);
#1079=FACE_OUTER_BOUND('',#1288,.T.);
#1080=FACE_OUTER_BOUND('',#1289,.T.);
#1081=FACE_OUTER_BOUND('',#1290,.T.);
#1082=FACE_OUTER_BOUND('',#1291,.T.);
#1083=FACE_OUTER_BOUND('',#1292,.T.);
#1084=FACE_OUTER_BOUND('',#1293,.T.);
#1085=FACE_OUTER_BOUND('',#1294,.T.);
#1086=FACE_OUTER_BOUND('',#1295,.T.);
#1087=FACE_OUTER_BOUND('',#1296,.T.);
#1088=FACE_OUTER_BOUND('',#1297,.T.);
#1089=FACE_OUTER_BOUND('',#1298,.T.);
#1090=FACE_OUTER_BOUND('',#1299,.T.);
#1091=FACE_OUTER_BOUND('',#1301,.T.);
#1092=FACE_OUTER_BOUND('',#1303,.T.);
#1093=FACE_OUTER_BOUND('',#1304,.T.);
#1094=FACE_OUTER_BOUND('',#1305,.T.);
#1095=FACE_OUTER_BOUND('',#1306,.T.);
#1096=FACE_OUTER_BOUND('',#1307,.T.);
#1097=FACE_OUTER_BOUND('',#1308,.T.);
#1098=FACE_OUTER_BOUND('',#1309,.T.);
#1099=FACE_OUTER_BOUND('',#1310,.T.);
#1100=FACE_OUTER_BOUND('',#1311,.T.);
#1101=FACE_OUTER_BOUND('',#1312,.T.);
#1102=FACE_OUTER_BOUND('',#1313,.T.);
#1103=FACE_OUTER_BOUND('',#1315,.T.);
#1104=FACE_OUTER_BOUND('',#1316,.T.);
#1105=FACE_OUTER_BOUND('',#1317,.T.);
#1106=FACE_OUTER_BOUND('',#1318,.T.);
#1107=FACE_OUTER_BOUND('',#1319,.T.);
#1108=FACE_OUTER_BOUND('',#1320,.T.);
#1109=FACE_OUTER_BOUND('',#1321,.T.);
#1110=FACE_OUTER_BOUND('',#1322,.T.);
#1111=FACE_OUTER_BOUND('',#1323,.T.);
#1112=FACE_OUTER_BOUND('',#1324,.T.);
#1113=FACE_OUTER_BOUND('',#1325,.T.);
#1114=FACE_OUTER_BOUND('',#1326,.T.);
#1115=FACE_OUTER_BOUND('',#1327,.T.);
#1116=FACE_OUTER_BOUND('',#1328,.T.);
#1117=FACE_OUTER_BOUND('',#1329,.T.);
#1118=FACE_OUTER_BOUND('',#1330,.T.);
#1119=FACE_OUTER_BOUND('',#1331,.T.);
#1120=FACE_OUTER_BOUND('',#1333,.T.);
#1121=FACE_OUTER_BOUND('',#1335,.T.);
#1122=FACE_OUTER_BOUND('',#1336,.T.);
#1123=FACE_OUTER_BOUND('',#1337,.T.);
#1124=FACE_OUTER_BOUND('',#1339,.T.);
#1125=FACE_OUTER_BOUND('',#1341,.T.);
#1126=FACE_OUTER_BOUND('',#1343,.T.);
#1127=FACE_OUTER_BOUND('',#1344,.T.);
#1128=FACE_OUTER_BOUND('',#1345,.T.);
#1129=FACE_OUTER_BOUND('',#1346,.T.);
#1130=FACE_OUTER_BOUND('',#1347,.T.);
#1131=FACE_OUTER_BOUND('',#1348,.T.);
#1132=FACE_OUTER_BOUND('',#1350,.T.);
#1133=FACE_OUTER_BOUND('',#1352,.T.);
#1134=FACE_OUTER_BOUND('',#1353,.T.);
#1135=FACE_OUTER_BOUND('',#1354,.T.);
#1136=FACE_OUTER_BOUND('',#1356,.T.);
#1137=FACE_OUTER_BOUND('',#1358,.T.);
#1138=FACE_OUTER_BOUND('',#1359,.T.);
#1139=FACE_OUTER_BOUND('',#1360,.T.);
#1140=FACE_OUTER_BOUND('',#1361,.T.);
#1141=FACE_OUTER_BOUND('',#1362,.T.);
#1142=FACE_OUTER_BOUND('',#1363,.T.);
#1143=FACE_OUTER_BOUND('',#1364,.T.);
#1144=FACE_OUTER_BOUND('',#1365,.T.);
#1145=FACE_OUTER_BOUND('',#1371,.T.);
#1146=FACE_OUTER_BOUND('',#1377,.T.);
#1147=FACE_OUTER_BOUND('',#1379,.T.);
#1148=FACE_OUTER_BOUND('',#1380,.T.);
#1149=FACE_OUTER_BOUND('',#1381,.T.);
#1150=FACE_OUTER_BOUND('',#1382,.T.);
#1151=FACE_OUTER_BOUND('',#1383,.T.);
#1152=FACE_OUTER_BOUND('',#1384,.T.);
#1153=FACE_OUTER_BOUND('',#1385,.T.);
#1154=FACE_OUTER_BOUND('',#1386,.T.);
#1155=FACE_OUTER_BOUND('',#1387,.T.);
#1156=FACE_OUTER_BOUND('',#1388,.T.);
#1157=FACE_OUTER_BOUND('',#1389,.T.);
#1158=FACE_OUTER_BOUND('',#1390,.T.);
#1159=FACE_OUTER_BOUND('',#1391,.T.);
#1160=FACE_OUTER_BOUND('',#1392,.T.);
#1161=FACE_OUTER_BOUND('',#1393,.T.);
#1162=FACE_OUTER_BOUND('',#1394,.T.);
#1163=FACE_OUTER_BOUND('',#1395,.T.);
#1164=FACE_OUTER_BOUND('',#1396,.T.);
#1165=FACE_OUTER_BOUND('',#1397,.T.);
#1166=FACE_OUTER_BOUND('',#1398,.T.);
#1167=FACE_OUTER_BOUND('',#1399,.T.);
#1168=FACE_OUTER_BOUND('',#1400,.T.);
#1169=FACE_OUTER_BOUND('',#1401,.T.);
#1170=FACE_OUTER_BOUND('',#1402,.T.);
#1171=FACE_OUTER_BOUND('',#1403,.T.);
#1172=FACE_OUTER_BOUND('',#1404,.T.);
#1173=FACE_OUTER_BOUND('',#1405,.T.);
#1174=FACE_OUTER_BOUND('',#1406,.T.);
#1175=FACE_OUTER_BOUND('',#1407,.T.);
#1176=FACE_OUTER_BOUND('',#1408,.T.);
#1177=FACE_OUTER_BOUND('',#1409,.T.);
#1178=FACE_OUTER_BOUND('',#1410,.T.);
#1179=FACE_OUTER_BOUND('',#1411,.T.);
#1180=FACE_OUTER_BOUND('',#1412,.T.);
#1181=FACE_OUTER_BOUND('',#1413,.T.);
#1182=FACE_OUTER_BOUND('',#1414,.T.);
#1183=FACE_OUTER_BOUND('',#1415,.T.);
#1184=FACE_OUTER_BOUND('',#1416,.T.);
#1185=FACE_OUTER_BOUND('',#1417,.T.);
#1186=FACE_OUTER_BOUND('',#1418,.T.);
#1187=FACE_OUTER_BOUND('',#1419,.T.);
#1188=FACE_OUTER_BOUND('',#1420,.T.);
#1189=EDGE_LOOP('',(#2402,#2403,#2404,#2405));
#1190=EDGE_LOOP('',(#2406,#2407,#2408,#2409));
#1191=EDGE_LOOP('',(#2410));
#1192=EDGE_LOOP('',(#2411));
#1193=EDGE_LOOP('',(#2412,#2413,#2414,#2415));
#1194=EDGE_LOOP('',(#2416));
#1195=EDGE_LOOP('',(#2417));
#1196=EDGE_LOOP('',(#2418,#2419,#2420,#2421));
#1197=EDGE_LOOP('',(#2422,#2423,#2424,#2425));
#1198=EDGE_LOOP('',(#2426,#2427,#2428,#2429,#2430,#2431,#2432,#2433));
#1199=EDGE_LOOP('',(#2434,#2435,#2436,#2437,#2438));
#1200=EDGE_LOOP('',(#2439,#2440,#2441,#2442,#2443,#2444,#2445,#2446,#2447,
#2448,#2449,#2450,#2451,#2452,#2453,#2454,#2455,#2456,#2457,#2458));
#1201=EDGE_LOOP('',(#2459,#2460,#2461,#2462));
#1202=EDGE_LOOP('',(#2463,#2464,#2465,#2466));
#1203=EDGE_LOOP('',(#2467,#2468,#2469,#2470));
#1204=EDGE_LOOP('',(#2471,#2472,#2473,#2474));
#1205=EDGE_LOOP('',(#2475,#2476,#2477,#2478));
#1206=EDGE_LOOP('',(#2479,#2480,#2481,#2482));
#1207=EDGE_LOOP('',(#2483,#2484,#2485,#2486));
#1208=EDGE_LOOP('',(#2487,#2488,#2489,#2490));
#1209=EDGE_LOOP('',(#2491,#2492,#2493,#2494));
#1210=EDGE_LOOP('',(#2495,#2496,#2497,#2498));
#1211=EDGE_LOOP('',(#2499,#2500,#2501,#2502));
#1212=EDGE_LOOP('',(#2503,#2504,#2505,#2506));
#1213=EDGE_LOOP('',(#2507,#2508,#2509,#2510));
#1214=EDGE_LOOP('',(#2511,#2512,#2513,#2514));
#1215=EDGE_LOOP('',(#2515,#2516,#2517,#2518));
#1216=EDGE_LOOP('',(#2519,#2520,#2521,#2522));
#1217=EDGE_LOOP('',(#2523,#2524,#2525,#2526));
#1218=EDGE_LOOP('',(#2527,#2528,#2529,#2530));
#1219=EDGE_LOOP('',(#2531,#2532,#2533,#2534));
#1220=EDGE_LOOP('',(#2535,#2536,#2537,#2538));
#1221=EDGE_LOOP('',(#2539,#2540,#2541,#2542));
#1222=EDGE_LOOP('',(#2543,#2544,#2545,#2546));
#1223=EDGE_LOOP('',(#2547,#2548,#2549,#2550));
#1224=EDGE_LOOP('',(#2551,#2552,#2553,#2554,#2555));
#1225=EDGE_LOOP('',(#2556,#2557,#2558,#2559,#2560,#2561,#2562));
#1226=EDGE_LOOP('',(#2563,#2564,#2565,#2566));
#1227=EDGE_LOOP('',(#2567,#2568,#2569,#2570));
#1228=EDGE_LOOP('',(#2571,#2572,#2573,#2574));
#1229=EDGE_LOOP('',(#2575,#2576,#2577,#2578));
#1230=EDGE_LOOP('',(#2579,#2580,#2581,#2582));
#1231=EDGE_LOOP('',(#2583,#2584,#2585,#2586));
#1232=EDGE_LOOP('',(#2587,#2588,#2589,#2590));
#1233=EDGE_LOOP('',(#2591,#2592,#2593,#2594,#2595));
#1234=EDGE_LOOP('',(#2596,#2597,#2598,#2599));
#1235=EDGE_LOOP('',(#2600,#2601,#2602,#2603));
#1236=EDGE_LOOP('',(#2604,#2605,#2606,#2607));
#1237=EDGE_LOOP('',(#2608,#2609,#2610,#2611));
#1238=EDGE_LOOP('',(#2612,#2613,#2614,#2615));
#1239=EDGE_LOOP('',(#2616,#2617,#2618,#2619));
#1240=EDGE_LOOP('',(#2620,#2621,#2622,#2623));
#1241=EDGE_LOOP('',(#2624,#2625,#2626,#2627));
#1242=EDGE_LOOP('',(#2628,#2629,#2630,#2631));
#1243=EDGE_LOOP('',(#2632,#2633,#2634,#2635));
#1244=EDGE_LOOP('',(#2636,#2637,#2638,#2639));
#1245=EDGE_LOOP('',(#2640,#2641,#2642,#2643));
#1246=EDGE_LOOP('',(#2644,#2645,#2646,#2647));
#1247=EDGE_LOOP('',(#2648,#2649,#2650,#2651));
#1248=EDGE_LOOP('',(#2652,#2653,#2654,#2655));
#1249=EDGE_LOOP('',(#2656,#2657,#2658,#2659,#2660));
#1250=EDGE_LOOP('',(#2661,#2662,#2663,#2664));
#1251=EDGE_LOOP('',(#2665,#2666,#2667,#2668,#2669));
#1252=EDGE_LOOP('',(#2670,#2671,#2672,#2673));
#1253=EDGE_LOOP('',(#2674,#2675,#2676,#2677,#2678));
#1254=EDGE_LOOP('',(#2679,#2680,#2681,#2682,#2683));
#1255=EDGE_LOOP('',(#2684,#2685,#2686,#2687));
#1256=EDGE_LOOP('',(#2688,#2689,#2690,#2691));
#1257=EDGE_LOOP('',(#2692,#2693,#2694,#2695));
#1258=EDGE_LOOP('',(#2696,#2697,#2698,#2699));
#1259=EDGE_LOOP('',(#2700,#2701,#2702,#2703));
#1260=EDGE_LOOP('',(#2704,#2705,#2706,#2707));
#1261=EDGE_LOOP('',(#2708,#2709,#2710,#2711));
#1262=EDGE_LOOP('',(#2712,#2713,#2714,#2715));
#1263=EDGE_LOOP('',(#2716,#2717,#2718,#2719));
#1264=EDGE_LOOP('',(#2720,#2721,#2722,#2723));
#1265=EDGE_LOOP('',(#2724,#2725,#2726,#2727));
#1266=EDGE_LOOP('',(#2728,#2729,#2730,#2731));
#1267=EDGE_LOOP('',(#2732,#2733,#2734,#2735));
#1268=EDGE_LOOP('',(#2736,#2737,#2738,#2739));
#1269=EDGE_LOOP('',(#2740,#2741,#2742,#2743));
#1270=EDGE_LOOP('',(#2744,#2745,#2746,#2747));
#1271=EDGE_LOOP('',(#2748,#2749,#2750,#2751));
#1272=EDGE_LOOP('',(#2752,#2753,#2754,#2755,#2756));
#1273=EDGE_LOOP('',(#2757,#2758,#2759,#2760,#2761));
#1274=EDGE_LOOP('',(#2762,#2763,#2764,#2765,#2766));
#1275=EDGE_LOOP('',(#2767,#2768,#2769,#2770,#2771));
#1276=EDGE_LOOP('',(#2772,#2773,#2774,#2775));
#1277=EDGE_LOOP('',(#2776,#2777,#2778,#2779));
#1278=EDGE_LOOP('',(#2780,#2781,#2782,#2783));
#1279=EDGE_LOOP('',(#2784,#2785,#2786,#2787));
#1280=EDGE_LOOP('',(#2788,#2789,#2790,#2791));
#1281=EDGE_LOOP('',(#2792,#2793,#2794,#2795));
#1282=EDGE_LOOP('',(#2796,#2797,#2798,#2799,#2800,#2801));
#1283=EDGE_LOOP('',(#2802,#2803,#2804,#2805,#2806));
#1284=EDGE_LOOP('',(#2807,#2808,#2809,#2810,#2811));
#1285=EDGE_LOOP('',(#2812,#2813,#2814,#2815));
#1286=EDGE_LOOP('',(#2816,#2817,#2818,#2819));
#1287=EDGE_LOOP('',(#2820,#2821,#2822,#2823,#2824));
#1288=EDGE_LOOP('',(#2825,#2826,#2827,#2828,#2829,#2830));
#1289=EDGE_LOOP('',(#2831,#2832,#2833,#2834));
#1290=EDGE_LOOP('',(#2835,#2836,#2837,#2838,#2839));
#1291=EDGE_LOOP('',(#2840,#2841,#2842,#2843,#2844,#2845,#2846,#2847,#2848));
#1292=EDGE_LOOP('',(#2849,#2850,#2851,#2852,#2853,#2854,#2855,#2856,#2857,
#2858));
#1293=EDGE_LOOP('',(#2859,#2860,#2861));
#1294=EDGE_LOOP('',(#2862,#2863,#2864));
#1295=EDGE_LOOP('',(#2865,#2866,#2867,#2868,#2869,#2870,#2871,#2872,#2873,
#2874));
#1296=EDGE_LOOP('',(#2875,#2876,#2877));
#1297=EDGE_LOOP('',(#2878,#2879,#2880,#2881,#2882,#2883));
#1298=EDGE_LOOP('',(#2884,#2885,#2886,#2887,#2888));
#1299=EDGE_LOOP('',(#2889));
#1300=EDGE_LOOP('',(#2890));
#1301=EDGE_LOOP('',(#2891));
#1302=EDGE_LOOP('',(#2892));
#1303=EDGE_LOOP('',(#2893,#2894,#2895,#2896,#2897,#2898,#2899,#2900,#2901,
#2902,#2903,#2904,#2905));
#1304=EDGE_LOOP('',(#2906,#2907,#2908,#2909,#2910,#2911,#2912,#2913,#2914,
#2915,#2916,#2917,#2918,#2919,#2920,#2921,#2922,#2923,#2924,#2925,#2926,
#2927));
#1305=EDGE_LOOP('',(#2928,#2929,#2930,#2931,#2932,#2933,#2934,#2935,#2936,
#2937,#2938,#2939,#2940,#2941,#2942,#2943,#2944,#2945,#2946,#2947,#2948,
#2949));
#1306=EDGE_LOOP('',(#2950,#2951,#2952,#2953,#2954,#2955,#2956,#2957,#2958,
#2959,#2960,#2961,#2962,#2963,#2964,#2965,#2966,#2967,#2968));
#1307=EDGE_LOOP('',(#2969,#2970,#2971,#2972,#2973,#2974,#2975,#2976,#2977,
#2978,#2979,#2980,#2981,#2982,#2983,#2984,#2985,#2986,#2987));
#1308=EDGE_LOOP('',(#2988,#2989,#2990,#2991,#2992,#2993,#2994,#2995,#2996,
#2997,#2998,#2999,#3000,#3001,#3002,#3003,#3004,#3005,#3006,#3007,#3008,
#3009,#3010,#3011,#3012,#3013));
#1309=EDGE_LOOP('',(#3014,#3015,#3016,#3017,#3018,#3019,#3020,#3021,#3022,
#3023,#3024,#3025,#3026,#3027,#3028,#3029,#3030,#3031,#3032,#3033,#3034,
#3035,#3036,#3037,#3038,#3039));
#1310=EDGE_LOOP('',(#3040,#3041,#3042,#3043,#3044,#3045,#3046,#3047,#3048,
#3049,#3050,#3051,#3052,#3053,#3054,#3055,#3056,#3057,#3058,#3059,#3060,
#3061,#3062,#3063,#3064));
#1311=EDGE_LOOP('',(#3065,#3066,#3067,#3068,#3069,#3070,#3071,#3072,#3073,
#3074,#3075,#3076,#3077,#3078,#3079,#3080,#3081,#3082,#3083,#3084,#3085,
#3086,#3087,#3088,#3089));
#1312=EDGE_LOOP('',(#3090,#3091,#3092,#3093));
#1313=EDGE_LOOP('',(#3094));
#1314=EDGE_LOOP('',(#3095));
#1315=EDGE_LOOP('',(#3096,#3097,#3098,#3099,#3100));
#1316=EDGE_LOOP('',(#3101,#3102,#3103,#3104));
#1317=EDGE_LOOP('',(#3105,#3106,#3107,#3108));
#1318=EDGE_LOOP('',(#3109,#3110,#3111,#3112));
#1319=EDGE_LOOP('',(#3113,#3114,#3115));
#1320=EDGE_LOOP('',(#3116,#3117,#3118,#3119,#3120,#3121));
#1321=EDGE_LOOP('',(#3122,#3123,#3124,#3125));
#1322=EDGE_LOOP('',(#3126,#3127,#3128,#3129,#3130));
#1323=EDGE_LOOP('',(#3131,#3132,#3133,#3134));
#1324=EDGE_LOOP('',(#3135,#3136,#3137,#3138));
#1325=EDGE_LOOP('',(#3139,#3140,#3141,#3142));
#1326=EDGE_LOOP('',(#3143,#3144,#3145,#3146));
#1327=EDGE_LOOP('',(#3147,#3148,#3149,#3150));
#1328=EDGE_LOOP('',(#3151,#3152,#3153,#3154));
#1329=EDGE_LOOP('',(#3155,#3156,#3157,#3158));
#1330=EDGE_LOOP('',(#3159,#3160,#3161,#3162,#3163,#3164,#3165,#3166,#3167,
#3168,#3169));
#1331=EDGE_LOOP('',(#3170));
#1332=EDGE_LOOP('',(#3171));
#1333=EDGE_LOOP('',(#3172));
#1334=EDGE_LOOP('',(#3173,#3174));
#1335=EDGE_LOOP('',(#3175,#3176,#3177,#3178));
#1336=EDGE_LOOP('',(#3179,#3180,#3181,#3182,#3183,#3184,#3185,#3186,#3187,
#3188,#3189,#3190));
#1337=EDGE_LOOP('',(#3191));
#1338=EDGE_LOOP('',(#3192));
#1339=EDGE_LOOP('',(#3193));
#1340=EDGE_LOOP('',(#3194,#3195,#3196,#3197));
#1341=EDGE_LOOP('',(#3198));
#1342=EDGE_LOOP('',(#3199));
#1343=EDGE_LOOP('',(#3200,#3201,#3202,#3203));
#1344=EDGE_LOOP('',(#3204));
#1345=EDGE_LOOP('',(#3205));
#1346=EDGE_LOOP('',(#3206,#3207,#3208,#3209));
#1347=EDGE_LOOP('',(#3210,#3211,#3212,#3213));
#1348=EDGE_LOOP('',(#3214));
#1349=EDGE_LOOP('',(#3215));
#1350=EDGE_LOOP('',(#3216));
#1351=EDGE_LOOP('',(#3217));
#1352=EDGE_LOOP('',(#3218,#3219,#3220,#3221));
#1353=EDGE_LOOP('',(#3222,#3223,#3224,#3225));
#1354=EDGE_LOOP('',(#3226));
#1355=EDGE_LOOP('',(#3227));
#1356=EDGE_LOOP('',(#3228));
#1357=EDGE_LOOP('',(#3229));
#1358=EDGE_LOOP('',(#3230,#3231,#3232,#3233));
#1359=EDGE_LOOP('',(#3234,#3235,#3236,#3237));
#1360=EDGE_LOOP('',(#3238,#3239,#3240,#3241));
#1361=EDGE_LOOP('',(#3242,#3243,#3244,#3245));
#1362=EDGE_LOOP('',(#3246,#3247,#3248,#3249));
#1363=EDGE_LOOP('',(#3250,#3251,#3252,#3253));
#1364=EDGE_LOOP('',(#3254,#3255,#3256,#3257));
#1365=EDGE_LOOP('',(#3258));
#1366=EDGE_LOOP('',(#3259));
#1367=EDGE_LOOP('',(#3260));
#1368=EDGE_LOOP('',(#3261));
#1369=EDGE_LOOP('',(#3262));
#1370=EDGE_LOOP('',(#3263));
#1371=EDGE_LOOP('',(#3264));
#1372=EDGE_LOOP('',(#3265));
#1373=EDGE_LOOP('',(#3266));
#1374=EDGE_LOOP('',(#3267));
#1375=EDGE_LOOP('',(#3268));
#1376=EDGE_LOOP('',(#3269));
#1377=EDGE_LOOP('',(#3270));
#1378=EDGE_LOOP('',(#3271));
#1379=EDGE_LOOP('',(#3272,#3273,#3274,#3275));
#1380=EDGE_LOOP('',(#3276,#3277,#3278,#3279));
#1381=EDGE_LOOP('',(#3280,#3281,#3282,#3283));
#1382=EDGE_LOOP('',(#3284,#3285,#3286,#3287));
#1383=EDGE_LOOP('',(#3288,#3289,#3290,#3291));
#1384=EDGE_LOOP('',(#3292,#3293,#3294,#3295));
#1385=EDGE_LOOP('',(#3296,#3297,#3298,#3299));
#1386=EDGE_LOOP('',(#3300,#3301,#3302));
#1387=EDGE_LOOP('',(#3303,#3304,#3305));
#1388=EDGE_LOOP('',(#3306,#3307,#3308,#3309));
#1389=EDGE_LOOP('',(#3310,#3311,#3312,#3313));
#1390=EDGE_LOOP('',(#3314,#3315,#3316,#3317));
#1391=EDGE_LOOP('',(#3318,#3319,#3320,#3321));
#1392=EDGE_LOOP('',(#3322,#3323,#3324,#3325));
#1393=EDGE_LOOP('',(#3326,#3327,#3328,#3329));
#1394=EDGE_LOOP('',(#3330,#3331,#3332));
#1395=EDGE_LOOP('',(#3333,#3334,#3335));
#1396=EDGE_LOOP('',(#3336,#3337,#3338));
#1397=EDGE_LOOP('',(#3339,#3340,#3341));
#1398=EDGE_LOOP('',(#3342,#3343,#3344,#3345));
#1399=EDGE_LOOP('',(#3346,#3347,#3348,#3349));
#1400=EDGE_LOOP('',(#3350,#3351,#3352,#3353));
#1401=EDGE_LOOP('',(#3354,#3355,#3356,#3357));
#1402=EDGE_LOOP('',(#3358,#3359,#3360));
#1403=EDGE_LOOP('',(#3361,#3362,#3363));
#1404=EDGE_LOOP('',(#3364,#3365,#3366,#3367));
#1405=EDGE_LOOP('',(#3368,#3369,#3370,#3371));
#1406=EDGE_LOOP('',(#3372));
#1407=EDGE_LOOP('',(#3373));
#1408=EDGE_LOOP('',(#3374,#3375,#3376,#3377));
#1409=EDGE_LOOP('',(#3378,#3379,#3380,#3381,#3382,#3383,#3384,#3385,#3386,
#3387));
#1410=EDGE_LOOP('',(#3388,#3389,#3390,#3391,#3392,#3393,#3394,#3395,#3396,
#3397,#3398,#3399,#3400,#3401));
#1411=EDGE_LOOP('',(#3402,#3403,#3404));
#1412=EDGE_LOOP('',(#3405,#3406));
#1413=EDGE_LOOP('',(#3407,#3408,#3409,#3410,#3411));
#1414=EDGE_LOOP('',(#3412,#3413,#3414,#3415));
#1415=EDGE_LOOP('',(#3416,#3417,#3418,#3419,#3420));
#1416=EDGE_LOOP('',(#3421,#3422,#3423,#3424));
#1417=EDGE_LOOP('',(#3425,#3426,#3427,#3428,#3429));
#1418=EDGE_LOOP('',(#3430,#3431,#3432,#3433,#3434));
#1419=EDGE_LOOP('',(#3435,#3436,#3437,#3438));
#1420=EDGE_LOOP('',(#3439));
#1421=CIRCLE('',#3799,3.96875);
#1422=CIRCLE('',#3800,146.03125);
#1423=CIRCLE('',#3803,3.96875);
#1424=CIRCLE('',#3804,3.96875);
#1425=CIRCLE('',#3809,3.96875);
#1426=CIRCLE('',#3810,3.96875);
#1427=CIRCLE('',#3815,40.);
#1428=CIRCLE('',#3816,40.);
#1429=CIRCLE('',#3818,46.);
#1430=CIRCLE('',#3819,46.);
#1431=CIRCLE('',#3821,40.);
#1432=CIRCLE('',#3822,40.);
#1433=CIRCLE('',#3823,40.);
#1434=CIRCLE('',#3824,40.);
#1435=CIRCLE('',#3826,3.96373117189689);
#1436=CIRCLE('',#3827,46.);
#1437=CIRCLE('',#3829,36.);
#1438=CIRCLE('',#3830,36.);
#1439=CIRCLE('',#3831,36.);
#1440=CIRCLE('',#3832,36.);
#1441=CIRCLE('',#3833,36.);
#1442=CIRCLE('',#3844,46.);
#1443=CIRCLE('',#3851,9169.15281567978);
#1444=CIRCLE('',#3852,9169.15281635233);
#1445=CIRCLE('',#3853,9169.15281632149);
#1446=CIRCLE('',#3854,9169.15281507871);
#1447=CIRCLE('',#3855,48.723191004622);
#1448=CIRCLE('',#3856,48.5934304680711);
#1449=CIRCLE('',#3857,9189.55754674609);
#1450=CIRCLE('',#3858,9189.55754816358);
#1451=CIRCLE('',#3859,9189.5575479708);
#1452=CIRCLE('',#3860,9189.55754886945);
#1453=CIRCLE('',#3861,15.8748636894354);
#1454=CIRCLE('',#3881,48.5937195834179);
#1455=CIRCLE('',#3882,9169.15281371648);
#1456=CIRCLE('',#3883,9189.55754697953);
#1457=CIRCLE('',#3884,9169.15281729791);
#1458=CIRCLE('',#3885,9189.55754810571);
#1459=CIRCLE('',#3886,9169.15281617656);
#1460=CIRCLE('',#3887,9189.55754697953);
#1461=CIRCLE('',#3888,9169.15281646739);
#1462=CIRCLE('',#3889,9189.55754853012);
#1463=CIRCLE('',#3891,48.5805105169702);
#1464=CIRCLE('',#3893,48.5805105169702);
#1465=CIRCLE('',#3895,46.);
#1466=CIRCLE('',#3902,9169.15281622634);
#1467=CIRCLE('',#3903,46.0136265696391);
#1468=CIRCLE('',#3907,48.7063293750001);
#1469=CIRCLE('',#3908,9169.15281512294);
#1470=CIRCLE('',#3916,46.);
#1471=CIRCLE('',#3934,47.293670625);
#1472=CIRCLE('',#3939,50.);
#1473=CIRCLE('',#3941,50.);
#1474=CIRCLE('',#3944,50.);
#1475=CIRCLE('',#3946,52.5);
#1476=CIRCLE('',#3947,52.5);
#1477=CIRCLE('',#3949,52.5);
#1478=CIRCLE('',#3950,52.5);
#1479=CIRCLE('',#3952,56.);
#1480=CIRCLE('',#3953,56.);
#1481=CIRCLE('',#3955,50.);
#1482=CIRCLE('',#3956,50.);
#1483=CIRCLE('',#3968,52.5);
#1484=CIRCLE('',#3969,52.5);
#1485=CIRCLE('',#3974,16.7);
#1486=CIRCLE('',#3975,16.7);
#1487=CIRCLE('',#3977,40.);
#1488=CIRCLE('',#3978,40.);
#1489=CIRCLE('',#3983,14.8);
#1490=CIRCLE('',#3984,14.8);
#1491=CIRCLE('',#3986,16.7);
#1492=CIRCLE('',#3987,16.7);
#1493=CIRCLE('',#3992,13.5);
#1494=CIRCLE('',#3993,13.5);
#1495=CIRCLE('',#3995,16.7);
#1496=CIRCLE('',#3996,16.7);
#1497=CIRCLE('',#3998,5.);
#1498=CIRCLE('',#3999,5.);
#1499=CIRCLE('',#4001,5.);
#1500=CIRCLE('',#4002,5.);
#1501=CIRCLE('',#4004,5.);
#1502=CIRCLE('',#4005,5.);
#1503=CIRCLE('',#4007,5.);
#1504=CIRCLE('',#4008,5.);
#1505=CIRCLE('',#4010,50.);
#1506=CIRCLE('',#4011,50.);
#1507=CIRCLE('',#4023,1.);
#1508=CIRCLE('',#4024,1.);
#1509=CIRCLE('',#4026,1.);
#1510=CIRCLE('',#4027,1.);
#1511=CIRCLE('',#4029,1.);
#1512=CIRCLE('',#4030,1.);
#1513=CIRCLE('',#4032,1.);
#1514=CIRCLE('',#4034,1.);
#1515=CIRCLE('',#4036,1.);
#1516=CIRCLE('',#4037,1.);
#1517=CIRCLE('',#4039,1.);
#1518=CIRCLE('',#4041,1.);
#1519=CIRCLE('',#4043,1.);
#1520=CIRCLE('',#4044,1.);
#1521=CIRCLE('',#4046,1.);
#1522=CIRCLE('',#4048,1.);
#1523=CIRCLE('',#4050,1.);
#1524=CIRCLE('',#4052,1.);
#1525=CIRCLE('',#4054,1.);
#1526=CIRCLE('',#4056,1.);
#1527=CIRCLE('',#4058,1.);
#1528=CIRCLE('',#4060,1.);
#1529=CIRCLE('',#4062,1.);
#1530=CIRCLE('',#4064,1.);
#1531=CIRCLE('',#4068,3.96875);
#1532=CIRCLE('',#4069,3.96875);
#1533=CIRCLE('',#4074,6.35000000000001);
#1534=CIRCLE('',#4075,7.35000000000003);
#1535=CIRCLE('',#4077,6.35000000000001);
#1536=CIRCLE('',#4078,6.35000000000001);
#1537=CIRCLE('',#4081,6.35000000000001);
#1538=CIRCLE('',#4083,7.93750000000001);
#1539=CIRCLE('',#4084,7.93750000000001);
#1540=CIRCLE('',#4085,7.93750000000001);
#1541=CIRCLE('',#4087,7.93750000000001);
#1542=CIRCLE('',#4089,7.93750000000001);
#1543=CIRCLE('',#4090,7.93750000000001);
#1544=CIRCLE('',#4092,153.96875);
#1545=CIRCLE('',#4094,146.03125);
#1546=VERTEX_POINT('',#4991);
#1547=VERTEX_POINT('',#4996);
#1548=VERTEX_POINT('',#4998);
#1549=VERTEX_POINT('',#5005);
#1550=VERTEX_POINT('',#5007);
#1551=VERTEX_POINT('',#5014);
#1552=VERTEX_POINT('',#5016);
#1553=VERTEX_POINT('',#5020);
#1554=VERTEX_POINT('',#5022);
#1555=VERTEX_POINT('',#5026);
#1556=VERTEX_POINT('',#5027);
#1557=VERTEX_POINT('',#5029);
#1558=VERTEX_POINT('',#5044);
#1559=VERTEX_POINT('',#5046);
#1560=VERTEX_POINT('',#5049);
#1561=VERTEX_POINT('',#5066);
#1562=VERTEX_POINT('',#5067);
#1563=VERTEX_POINT('',#5086);
#1564=VERTEX_POINT('',#5088);
#1565=VERTEX_POINT('',#5090);
#1566=VERTEX_POINT('',#5099);
#1567=VERTEX_POINT('',#5100);
#1568=VERTEX_POINT('',#5119);
#1569=VERTEX_POINT('',#5121);
#1570=VERTEX_POINT('',#5123);
#1571=VERTEX_POINT('',#5125);
#1572=VERTEX_POINT('',#5144);
#1573=VERTEX_POINT('',#5146);
#1574=VERTEX_POINT('',#5148);
#1575=VERTEX_POINT('',#5150);
#1576=VERTEX_POINT('',#5163);
#1577=VERTEX_POINT('',#5166);
#1578=VERTEX_POINT('',#5177);
#1579=VERTEX_POINT('',#5179);
#1580=VERTEX_POINT('',#5181);
#1581=VERTEX_POINT('',#5183);
#1582=VERTEX_POINT('',#5202);
#1583=VERTEX_POINT('',#5204);
#1584=VERTEX_POINT('',#5208);
#1585=VERTEX_POINT('',#5209);
#1586=VERTEX_POINT('',#5211);
#1587=VERTEX_POINT('',#5219);
#1588=VERTEX_POINT('',#5229);
#1589=VERTEX_POINT('',#5230);
#1590=VERTEX_POINT('',#5232);
#1591=VERTEX_POINT('',#5240);
#1592=VERTEX_POINT('',#5253);
#1593=VERTEX_POINT('',#5254);
#1594=VERTEX_POINT('',#5256);
#1595=VERTEX_POINT('',#5264);
#1596=VERTEX_POINT('',#5274);
#1597=VERTEX_POINT('',#5275);
#1598=VERTEX_POINT('',#5277);
#1599=VERTEX_POINT('',#5285);
#1600=VERTEX_POINT('',#5295);
#1601=VERTEX_POINT('',#5296);
#1602=VERTEX_POINT('',#5298);
#1603=VERTEX_POINT('',#5306);
#1604=VERTEX_POINT('',#5316);
#1605=VERTEX_POINT('',#5317);
#1606=VERTEX_POINT('',#5319);
#1607=VERTEX_POINT('',#5327);
#1608=VERTEX_POINT('',#5337);
#1609=VERTEX_POINT('',#5338);
#1610=VERTEX_POINT('',#5340);
#1611=VERTEX_POINT('',#5348);
#1612=VERTEX_POINT('',#5358);
#1613=VERTEX_POINT('',#5359);
#1614=VERTEX_POINT('',#5361);
#1615=VERTEX_POINT('',#5369);
#1616=VERTEX_POINT('',#5379);
#1617=VERTEX_POINT('',#5380);
#1618=VERTEX_POINT('',#5382);
#1619=VERTEX_POINT('',#5390);
#1620=VERTEX_POINT('',#5400);
#1621=VERTEX_POINT('',#5401);
#1622=VERTEX_POINT('',#5403);
#1623=VERTEX_POINT('',#5411);
#1624=VERTEX_POINT('',#5415);
#1625=VERTEX_POINT('',#5416);
#1626=VERTEX_POINT('',#5418);
#1627=VERTEX_POINT('',#5426);
#1628=VERTEX_POINT('',#5436);
#1629=VERTEX_POINT('',#5437);
#1630=VERTEX_POINT('',#5439);
#1631=VERTEX_POINT('',#5447);
#1632=VERTEX_POINT('',#5457);
#1633=VERTEX_POINT('',#5458);
#1634=VERTEX_POINT('',#5460);
#1635=VERTEX_POINT('',#5468);
#1636=VERTEX_POINT('',#5478);
#1637=VERTEX_POINT('',#5479);
#1638=VERTEX_POINT('',#5481);
#1639=VERTEX_POINT('',#5489);
#1640=VERTEX_POINT('',#5499);
#1641=VERTEX_POINT('',#5500);
#1642=VERTEX_POINT('',#5502);
#1643=VERTEX_POINT('',#5510);
#1644=VERTEX_POINT('',#5520);
#1645=VERTEX_POINT('',#5521);
#1646=VERTEX_POINT('',#5523);
#1647=VERTEX_POINT('',#5531);
#1648=VERTEX_POINT('',#5830);
#1649=VERTEX_POINT('',#5831);
#1650=VERTEX_POINT('',#6137);
#1651=VERTEX_POINT('',#6145);
#1652=VERTEX_POINT('',#6452);
#1653=VERTEX_POINT('',#6453);
#1654=VERTEX_POINT('',#6759);
#1655=VERTEX_POINT('',#6767);
#1656=VERTEX_POINT('',#7074);
#1657=VERTEX_POINT('',#7075);
#1658=VERTEX_POINT('',#7381);
#1659=VERTEX_POINT('',#7389);
#1660=VERTEX_POINT('',#7696);
#1661=VERTEX_POINT('',#7697);
#1662=VERTEX_POINT('',#8003);
#1663=VERTEX_POINT('',#8011);
#1664=VERTEX_POINT('',#8019);
#1665=VERTEX_POINT('',#8321);
#1666=VERTEX_POINT('',#8329);
#1667=VERTEX_POINT('',#8331);
#1668=VERTEX_POINT('',#8333);
#1669=VERTEX_POINT('',#8335);
#1670=VERTEX_POINT('',#8634);
#1671=VERTEX_POINT('',#8642);
#1672=VERTEX_POINT('',#8941);
#1673=VERTEX_POINT('',#8942);
#1674=VERTEX_POINT('',#9256);
#1675=VERTEX_POINT('',#9264);
#1676=VERTEX_POINT('',#9563);
#1677=VERTEX_POINT('',#9564);
#1678=VERTEX_POINT('',#9878);
#1679=VERTEX_POINT('',#9886);
#1680=VERTEX_POINT('',#10185);
#1681=VERTEX_POINT('',#10186);
#1682=VERTEX_POINT('',#10500);
#1683=VERTEX_POINT('',#10501);
#1684=VERTEX_POINT('',#10509);
#1685=VERTEX_POINT('',#10517);
#1686=VERTEX_POINT('',#10821);
#1687=VERTEX_POINT('',#10822);
#1688=VERTEX_POINT('',#10830);
#1689=VERTEX_POINT('',#10840);
#1690=VERTEX_POINT('',#10848);
#1691=VERTEX_POINT('',#10857);
#1692=VERTEX_POINT('',#10858);
#1693=VERTEX_POINT('',#10869);
#1694=VERTEX_POINT('',#10871);
#1695=VERTEX_POINT('',#10881);
#1696=VERTEX_POINT('',#10882);
#1697=VERTEX_POINT('',#10893);
#1698=VERTEX_POINT('',#10895);
#1699=VERTEX_POINT('',#10905);
#1700=VERTEX_POINT('',#10906);
#1701=VERTEX_POINT('',#10917);
#1702=VERTEX_POINT('',#10919);
#1703=VERTEX_POINT('',#10929);
#1704=VERTEX_POINT('',#10930);
#1705=VERTEX_POINT('',#10941);
#1706=VERTEX_POINT('',#10943);
#1707=VERTEX_POINT('',#10953);
#1708=VERTEX_POINT('',#10955);
#1709=VERTEX_POINT('',#10965);
#1710=VERTEX_POINT('',#10967);
#1711=VERTEX_POINT('',#10977);
#1712=VERTEX_POINT('',#10978);
#1713=VERTEX_POINT('',#10989);
#1714=VERTEX_POINT('',#10991);
#1715=VERTEX_POINT('',#11001);
#1716=VERTEX_POINT('',#11002);
#1717=VERTEX_POINT('',#11013);
#1718=VERTEX_POINT('',#11015);
#1719=VERTEX_POINT('',#11025);
#1720=VERTEX_POINT('',#11026);
#1721=VERTEX_POINT('',#11037);
#1722=VERTEX_POINT('',#11039);
#1723=VERTEX_POINT('',#11047);
#1724=VERTEX_POINT('',#11054);
#1725=VERTEX_POINT('',#11055);
#1726=VERTEX_POINT('',#11066);
#1727=VERTEX_POINT('',#11067);
#1728=VERTEX_POINT('',#11075);
#1729=VERTEX_POINT('',#11077);
#1730=VERTEX_POINT('',#11085);
#1731=VERTEX_POINT('',#11092);
#1732=VERTEX_POINT('',#11093);
#1733=VERTEX_POINT('',#11101);
#1734=VERTEX_POINT('',#11103);
#1735=VERTEX_POINT('',#11407);
#1736=VERTEX_POINT('',#11408);
#1737=VERTEX_POINT('',#11427);
#1738=VERTEX_POINT('',#11720);
#1739=VERTEX_POINT('',#11730);
#1740=VERTEX_POINT('',#11737);
#1741=VERTEX_POINT('',#13876);
#1742=VERTEX_POINT('',#13878);
#1743=VERTEX_POINT('',#16884);
#1744=VERTEX_POINT('',#16889);
#1745=VERTEX_POINT('',#16894);
#1746=VERTEX_POINT('',#16904);
#1747=VERTEX_POINT('',#16905);
#1748=VERTEX_POINT('',#16907);
#1749=VERTEX_POINT('',#16921);
#1750=VERTEX_POINT('',#16937);
#1751=VERTEX_POINT('',#16938);
#1752=VERTEX_POINT('',#16940);
#1753=VERTEX_POINT('',#16948);
#1754=VERTEX_POINT('',#16973);
#1755=VERTEX_POINT('',#16975);
#1756=VERTEX_POINT('',#16997);
#1757=VERTEX_POINT('',#16999);
#1758=VERTEX_POINT('',#17598);
#1759=VERTEX_POINT('',#17599);
#1760=VERTEX_POINT('',#17943);
#1761=VERTEX_POINT('',#17944);
#1762=VERTEX_POINT('',#17958);
#1763=VERTEX_POINT('',#18263);
#1764=VERTEX_POINT('',#18264);
#1765=VERTEX_POINT('',#18271);
#1766=VERTEX_POINT('',#18273);
#1767=VERTEX_POINT('',#18285);
#1768=VERTEX_POINT('',#18308);
#1769=VERTEX_POINT('',#18309);
#1770=VERTEX_POINT('',#18325);
#1771=VERTEX_POINT('',#18326);
#1772=VERTEX_POINT('',#18343);
#1773=VERTEX_POINT('',#18345);
#1774=VERTEX_POINT('',#18359);
#1775=VERTEX_POINT('',#19296);
#1776=VERTEX_POINT('',#19321);
#1777=VERTEX_POINT('',#19353);
#1778=VERTEX_POINT('',#19354);
#1779=VERTEX_POINT('',#19356);
#1780=VERTEX_POINT('',#19360);
#1781=VERTEX_POINT('',#19362);
#1782=VERTEX_POINT('',#19374);
#1783=VERTEX_POINT('',#19375);
#1784=VERTEX_POINT('',#19428);
#1785=VERTEX_POINT('',#19429);
#1786=VERTEX_POINT('',#19482);
#1787=VERTEX_POINT('',#19483);
#1788=VERTEX_POINT('',#19485);
#1789=VERTEX_POINT('',#19499);
#1790=VERTEX_POINT('',#19515);
#1791=VERTEX_POINT('',#19516);
#1792=VERTEX_POINT('',#19518);
#1793=VERTEX_POINT('',#19549);
#1794=VERTEX_POINT('',#19550);
#1795=VERTEX_POINT('',#19552);
#1796=VERTEX_POINT('',#19620);
#1797=VERTEX_POINT('',#19621);
#1798=VERTEX_POINT('',#19700);
#1799=VERTEX_POINT('',#19701);
#1800=VERTEX_POINT('',#19703);
#1801=VERTEX_POINT('',#19722);
#1802=VERTEX_POINT('',#19724);
#1803=VERTEX_POINT('',#19747);
#1804=VERTEX_POINT('',#19749);
#1805=VERTEX_POINT('',#19753);
#1806=VERTEX_POINT('',#19755);
#1807=VERTEX_POINT('',#19759);
#1808=VERTEX_POINT('',#19761);
#1809=VERTEX_POINT('',#19765);
#1810=VERTEX_POINT('',#19767);
#1811=VERTEX_POINT('',#20301);
#1812=VERTEX_POINT('',#20303);
#1813=VERTEX_POINT('',#20310);
#1814=VERTEX_POINT('',#20312);
#1815=VERTEX_POINT('',#20316);
#1816=VERTEX_POINT('',#20318);
#1817=VERTEX_POINT('',#20325);
#1818=VERTEX_POINT('',#20327);
#1819=VERTEX_POINT('',#20331);
#1820=VERTEX_POINT('',#20333);
#1821=VERTEX_POINT('',#20340);
#1822=VERTEX_POINT('',#20342);
#1823=VERTEX_POINT('',#20346);
#1824=VERTEX_POINT('',#20348);
#1825=VERTEX_POINT('',#20352);
#1826=VERTEX_POINT('',#20354);
#1827=VERTEX_POINT('',#20358);
#1828=VERTEX_POINT('',#20360);
#1829=VERTEX_POINT('',#20364);
#1830=VERTEX_POINT('',#20366);
#1831=VERTEX_POINT('',#20370);
#1832=VERTEX_POINT('',#20372);
#1833=VERTEX_POINT('',#20376);
#1834=VERTEX_POINT('',#20378);
#1835=VERTEX_POINT('',#20386);
#1836=VERTEX_POINT('',#20387);
#1837=VERTEX_POINT('',#20389);
#1838=VERTEX_POINT('',#20391);
#1839=VERTEX_POINT('',#20395);
#1840=VERTEX_POINT('',#20396);
#1841=VERTEX_POINT('',#20398);
#1842=VERTEX_POINT('',#20400);
#1843=VERTEX_POINT('',#20404);
#1844=VERTEX_POINT('',#20405);
#1845=VERTEX_POINT('',#20407);
#1846=VERTEX_POINT('',#20409);
#1847=VERTEX_POINT('',#20413);
#1848=VERTEX_POINT('',#20414);
#1849=VERTEX_POINT('',#20416);
#1850=VERTEX_POINT('',#20418);
#1851=VERTEX_POINT('',#20422);
#1852=VERTEX_POINT('',#20423);
#1853=VERTEX_POINT('',#20425);
#1854=VERTEX_POINT('',#20427);
#1855=VERTEX_POINT('',#20431);
#1856=VERTEX_POINT('',#20432);
#1857=VERTEX_POINT('',#20434);
#1858=VERTEX_POINT('',#20436);
#1859=VERTEX_POINT('',#20485);
#1860=VERTEX_POINT('',#20487);
#1861=VERTEX_POINT('',#20494);
#1862=VERTEX_POINT('',#20495);
#1863=VERTEX_POINT('',#20497);
#1864=VERTEX_POINT('',#20501);
#1865=VERTEX_POINT('',#20507);
#1866=VERTEX_POINT('',#20509);
#1867=VERTEX_POINT('',#20511);
#1868=VERTEX_POINT('',#20513);
#1869=VERTEX_POINT('',#20516);
#1870=VERTEX_POINT('',#20518);
#1871=VERTEX_POINT('',#20522);
#1872=VERTEX_POINT('',#20523);
#1873=VERTEX_POINT('',#20525);
#1874=VERTEX_POINT('',#20548);
#1875=VERTEX_POINT('',#20550);
#1876=VERTEX_POINT('',#20552);
#1877=VERTEX_POINT('',#20554);
#1878=VERTEX_POINT('',#20556);
#1879=VERTEX_POINT('',#20558);
#1880=VERTEX_POINT('',#20560);
#1881=VERTEX_POINT('',#20562);
#1882=VERTEX_POINT('',#20565);
#1883=EDGE_CURVE('',#1546,#1546,#1421,.T.);
#1884=EDGE_CURVE('',#1546,#1546,#1422,.T.);
#1885=EDGE_CURVE('',#1547,#1547,#1423,.T.);
#1886=EDGE_CURVE('',#1547,#1548,#448,.T.);
#1887=EDGE_CURVE('',#1548,#1548,#1424,.T.);
#1888=EDGE_CURVE('',#1549,#1549,#1425,.T.);
#1889=EDGE_CURVE('',#1549,#1550,#449,.T.);
#1890=EDGE_CURVE('',#1550,#1550,#1426,.T.);
#1891=EDGE_CURVE('',#1551,#1551,#1427,.T.);
#1892=EDGE_CURVE('',#1551,#1552,#450,.T.);
#1893=EDGE_CURVE('',#1552,#1552,#1428,.T.);
#1894=EDGE_CURVE('',#1553,#1553,#1429,.T.);
#1895=EDGE_CURVE('',#1553,#1554,#451,.T.);
#1896=EDGE_CURVE('',#1554,#1554,#1430,.T.);
#1897=EDGE_CURVE('',#1555,#1556,#1431,.T.);
#1898=EDGE_CURVE('',#1557,#1556,#294,.T.);
#1899=EDGE_CURVE('',#1557,#1558,#1432,.T.);
#1900=EDGE_CURVE('',#1558,#1559,#452,.T.);
#1901=EDGE_CURVE('',#1559,#1559,#1433,.T.);
#1902=EDGE_CURVE('',#1558,#1560,#1434,.T.);
#1903=EDGE_CURVE('',#1555,#1560,#295,.T.);
#1904=EDGE_CURVE('',#1561,#1562,#296,.T.);
#1905=EDGE_CURVE('',#1563,#1562,#1435,.T.);
#1906=EDGE_CURVE('',#1564,#1563,#1436,.T.);
#1907=EDGE_CURVE('',#1565,#1564,#297,.T.);
#1908=EDGE_CURVE('',#1561,#1565,#453,.T.);
#1909=EDGE_CURVE('',#1566,#1567,#298,.F.);
#1910=EDGE_CURVE('',#1567,#1568,#454,.T.);
#1911=EDGE_CURVE('',#1568,#1569,#1437,.T.);
#1912=EDGE_CURVE('',#1569,#1570,#455,.T.);
#1913=EDGE_CURVE('',#1570,#1571,#299,.T.);
#1914=EDGE_CURVE('',#1571,#1572,#456,.T.);
#1915=EDGE_CURVE('',#1572,#1573,#1438,.T.);
#1916=EDGE_CURVE('',#1573,#1574,#457,.T.);
#1917=EDGE_CURVE('',#1574,#1575,#300,.T.);
#1918=EDGE_CURVE('',#1575,#1576,#458,.T.);
#1919=EDGE_CURVE('',#1576,#1576,#1439,.T.);
#1920=EDGE_CURVE('',#1575,#1577,#301,.T.);
#1921=EDGE_CURVE('',#1577,#1578,#459,.T.);
#1922=EDGE_CURVE('',#1578,#1579,#1440,.T.);
#1923=EDGE_CURVE('',#1579,#1580,#460,.T.);
#1924=EDGE_CURVE('',#1580,#1581,#302,.T.);
#1925=EDGE_CURVE('',#1581,#1582,#461,.T.);
#1926=EDGE_CURVE('',#1582,#1583,#1441,.T.);
#1927=EDGE_CURVE('',#1583,#1566,#462,.T.);
#1928=EDGE_CURVE('',#1584,#1585,#463,.T.);
#1929=EDGE_CURVE('',#1586,#1584,#197,.T.);
#1930=EDGE_CURVE('',#1587,#1586,#464,.T.);
#1931=EDGE_CURVE('',#1587,#1585,#198,.T.);
#1932=EDGE_CURVE('',#1588,#1589,#465,.T.);
#1933=EDGE_CURVE('',#1588,#1590,#199,.T.);
#1934=EDGE_CURVE('',#1591,#1590,#303,.T.);
#1935=EDGE_CURVE('',#1589,#1591,#200,.T.);
#1936=EDGE_CURVE('',#1592,#1593,#466,.T.);
#1937=EDGE_CURVE('',#1594,#1592,#201,.T.);
#1938=EDGE_CURVE('',#1595,#1594,#467,.T.);
#1939=EDGE_CURVE('',#1595,#1593,#202,.T.);
#1940=EDGE_CURVE('',#1596,#1597,#468,.T.);
#1941=EDGE_CURVE('',#1596,#1598,#203,.T.);
#1942=EDGE_CURVE('',#1599,#1598,#469,.T.);
#1943=EDGE_CURVE('',#1597,#1599,#204,.T.);
#1944=EDGE_CURVE('',#1600,#1601,#470,.T.);
#1945=EDGE_CURVE('',#1602,#1600,#205,.T.);
#1946=EDGE_CURVE('',#1603,#1602,#471,.T.);
#1947=EDGE_CURVE('',#1603,#1601,#206,.T.);
#1948=EDGE_CURVE('',#1604,#1605,#472,.T.);
#1949=EDGE_CURVE('',#1604,#1606,#207,.T.);
#1950=EDGE_CURVE('',#1607,#1606,#473,.T.);
#1951=EDGE_CURVE('',#1605,#1607,#208,.T.);
#1952=EDGE_CURVE('',#1608,#1609,#474,.T.);
#1953=EDGE_CURVE('',#1610,#1608,#209,.T.);
#1954=EDGE_CURVE('',#1611,#1610,#475,.T.);
#1955=EDGE_CURVE('',#1611,#1609,#210,.T.);
#1956=EDGE_CURVE('',#1612,#1613,#476,.T.);
#1957=EDGE_CURVE('',#1612,#1614,#211,.T.);
#1958=EDGE_CURVE('',#1615,#1614,#477,.T.);
#1959=EDGE_CURVE('',#1613,#1615,#212,.T.);
#1960=EDGE_CURVE('',#1616,#1617,#478,.T.);
#1961=EDGE_CURVE('',#1616,#1618,#213,.T.);
#1962=EDGE_CURVE('',#1619,#1618,#479,.T.);
#1963=EDGE_CURVE('',#1617,#1619,#214,.T.);
#1964=EDGE_CURVE('',#1620,#1621,#480,.T.);
#1965=EDGE_CURVE('',#1622,#1620,#215,.T.);
#1966=EDGE_CURVE('',#1623,#1622,#481,.T.);
#1967=EDGE_CURVE('',#1621,#1623,#1442,.T.);
#1968=EDGE_CURVE('',#1624,#1625,#482,.T.);
#1969=EDGE_CURVE('',#1624,#1626,#216,.T.);
#1970=EDGE_CURVE('',#1627,#1626,#483,.T.);
#1971=EDGE_CURVE('',#1625,#1627,#217,.T.);
#1972=EDGE_CURVE('',#1628,#1629,#484,.T.);
#1973=EDGE_CURVE('',#1630,#1628,#218,.T.);
#1974=EDGE_CURVE('',#1631,#1630,#485,.T.);
#1975=EDGE_CURVE('',#1631,#1629,#219,.T.);
#1976=EDGE_CURVE('',#1632,#1633,#486,.T.);
#1977=EDGE_CURVE('',#1632,#1634,#220,.T.);
#1978=EDGE_CURVE('',#1635,#1634,#487,.T.);
#1979=EDGE_CURVE('',#1633,#1635,#221,.T.);
#1980=EDGE_CURVE('',#1636,#1637,#488,.T.);
#1981=EDGE_CURVE('',#1638,#1636,#222,.T.);
#1982=EDGE_CURVE('',#1639,#1638,#489,.T.);
#1983=EDGE_CURVE('',#1639,#1637,#223,.T.);
#1984=EDGE_CURVE('',#1640,#1641,#490,.T.);
#1985=EDGE_CURVE('',#1640,#1642,#224,.T.);
#1986=EDGE_CURVE('',#1643,#1642,#491,.T.);
#1987=EDGE_CURVE('',#1641,#1643,#225,.T.);
#1988=EDGE_CURVE('',#1644,#1645,#492,.T.);
#1989=EDGE_CURVE('',#1646,#1644,#226,.T.);
#1990=EDGE_CURVE('',#1647,#1646,#493,.T.);
#1991=EDGE_CURVE('',#1647,#1645,#227,.T.);
#1992=EDGE_CURVE('',#1648,#1649,#228,.T.);
#1993=EDGE_CURVE('',#1649,#1593,#1443,.T.);
#1994=EDGE_CURVE('',#1595,#1648,#304,.T.);
#1995=EDGE_CURVE('',#1596,#1650,#305,.T.);
#1996=EDGE_CURVE('',#1650,#1651,#229,.T.);
#1997=EDGE_CURVE('',#1651,#1598,#306,.T.);
#1998=EDGE_CURVE('',#1652,#1653,#230,.T.);
#1999=EDGE_CURVE('',#1653,#1601,#1444,.T.);
#2000=EDGE_CURVE('',#1603,#1652,#307,.T.);
#2001=EDGE_CURVE('',#1604,#1654,#308,.T.);
#2002=EDGE_CURVE('',#1654,#1655,#231,.T.);
#2003=EDGE_CURVE('',#1655,#1606,#309,.T.);
#2004=EDGE_CURVE('',#1656,#1657,#232,.T.);
#2005=EDGE_CURVE('',#1657,#1609,#1445,.T.);
#2006=EDGE_CURVE('',#1611,#1656,#310,.T.);
#2007=EDGE_CURVE('',#1612,#1658,#311,.T.);
#2008=EDGE_CURVE('',#1658,#1659,#233,.T.);
#2009=EDGE_CURVE('',#1659,#1614,#312,.T.);
#2010=EDGE_CURVE('',#1660,#1661,#234,.T.);
#2011=EDGE_CURVE('',#1661,#1585,#1446,.T.);
#2012=EDGE_CURVE('',#1587,#1660,#313,.T.);
#2013=EDGE_CURVE('',#1588,#1662,#314,.T.);
#2014=EDGE_CURVE('',#1662,#1663,#235,.T.);
#2015=EDGE_CURVE('',#1663,#1664,#315,.T.);
#2016=EDGE_CURVE('',#1664,#1590,#494,.T.);
#2017=EDGE_CURVE('',#1616,#1665,#316,.T.);
#2018=EDGE_CURVE('',#1665,#1666,#1447,.T.);
#2019=EDGE_CURVE('',#1666,#1667,#1448,.T.);
#2020=EDGE_CURVE('',#1667,#1668,#495,.T.);
#2021=EDGE_CURVE('',#1668,#1669,#236,.T.);
#2022=EDGE_CURVE('',#1669,#1618,#1449,.T.);
#2023=EDGE_CURVE('',#1624,#1670,#317,.T.);
#2024=EDGE_CURVE('',#1670,#1671,#237,.T.);
#2025=EDGE_CURVE('',#1671,#1626,#1450,.T.);
#2026=EDGE_CURVE('',#1672,#1673,#238,.T.);
#2027=EDGE_CURVE('',#1673,#1629,#318,.T.);
#2028=EDGE_CURVE('',#1631,#1672,#319,.T.);
#2029=EDGE_CURVE('',#1632,#1674,#320,.T.);
#2030=EDGE_CURVE('',#1674,#1675,#239,.T.);
#2031=EDGE_CURVE('',#1675,#1634,#1451,.T.);
#2032=EDGE_CURVE('',#1676,#1677,#240,.T.);
#2033=EDGE_CURVE('',#1677,#1637,#321,.T.);
#2034=EDGE_CURVE('',#1639,#1676,#322,.T.);
#2035=EDGE_CURVE('',#1640,#1678,#323,.T.);
#2036=EDGE_CURVE('',#1678,#1679,#241,.T.);
#2037=EDGE_CURVE('',#1679,#1642,#1452,.T.);
#2038=EDGE_CURVE('',#1680,#1681,#242,.T.);
#2039=EDGE_CURVE('',#1681,#1645,#324,.T.);
#2040=EDGE_CURVE('',#1647,#1680,#325,.T.);
#2041=EDGE_CURVE('',#1682,#1683,#243,.T.);
#2042=EDGE_CURVE('',#1682,#1684,#326,.T.);
#2043=EDGE_CURVE('',#1684,#1685,#244,.T.);
#2044=EDGE_CURVE('',#1685,#1683,#327,.T.);
#2045=EDGE_CURVE('',#1686,#1687,#245,.T.);
#2046=EDGE_CURVE('',#1687,#1688,#328,.T.);
#2047=EDGE_CURVE('',#1689,#1688,#246,.T.);
#2048=EDGE_CURVE('',#1689,#1690,#1453,.T.);
#2049=EDGE_CURVE('',#1690,#1686,#329,.T.);
#2050=EDGE_CURVE('',#1691,#1692,#247,.T.);
#2051=EDGE_CURVE('',#1692,#1649,#496,.T.);
#2052=EDGE_CURVE('',#1648,#1691,#497,.T.);
#2053=EDGE_CURVE('',#1650,#1693,#498,.T.);
#2054=EDGE_CURVE('',#1693,#1694,#248,.T.);
#2055=EDGE_CURVE('',#1694,#1651,#499,.T.);
#2056=EDGE_CURVE('',#1695,#1696,#249,.T.);
#2057=EDGE_CURVE('',#1696,#1653,#500,.T.);
#2058=EDGE_CURVE('',#1652,#1695,#501,.T.);
#2059=EDGE_CURVE('',#1654,#1697,#502,.T.);
#2060=EDGE_CURVE('',#1697,#1698,#250,.T.);
#2061=EDGE_CURVE('',#1698,#1655,#503,.T.);
#2062=EDGE_CURVE('',#1699,#1700,#251,.T.);
#2063=EDGE_CURVE('',#1700,#1657,#504,.T.);
#2064=EDGE_CURVE('',#1656,#1699,#505,.T.);
#2065=EDGE_CURVE('',#1658,#1701,#506,.T.);
#2066=EDGE_CURVE('',#1701,#1702,#252,.T.);
#2067=EDGE_CURVE('',#1702,#1659,#507,.T.);
#2068=EDGE_CURVE('',#1703,#1704,#253,.T.);
#2069=EDGE_CURVE('',#1704,#1661,#508,.T.);
#2070=EDGE_CURVE('',#1660,#1703,#509,.T.);
#2071=EDGE_CURVE('',#1662,#1705,#510,.T.);
#2072=EDGE_CURVE('',#1705,#1706,#254,.T.);
#2073=EDGE_CURVE('',#1706,#1663,#511,.T.);
#2074=EDGE_CURVE('',#1668,#1707,#512,.T.);
#2075=EDGE_CURVE('',#1707,#1708,#255,.T.);
#2076=EDGE_CURVE('',#1708,#1669,#513,.T.);
#2077=EDGE_CURVE('',#1670,#1709,#514,.T.);
#2078=EDGE_CURVE('',#1709,#1710,#256,.T.);
#2079=EDGE_CURVE('',#1710,#1671,#515,.T.);
#2080=EDGE_CURVE('',#1711,#1712,#257,.T.);
#2081=EDGE_CURVE('',#1712,#1673,#516,.T.);
#2082=EDGE_CURVE('',#1672,#1711,#517,.T.);
#2083=EDGE_CURVE('',#1674,#1713,#518,.T.);
#2084=EDGE_CURVE('',#1713,#1714,#258,.T.);
#2085=EDGE_CURVE('',#1714,#1675,#519,.T.);
#2086=EDGE_CURVE('',#1715,#1716,#259,.T.);
#2087=EDGE_CURVE('',#1716,#1677,#520,.T.);
#2088=EDGE_CURVE('',#1676,#1715,#521,.T.);
#2089=EDGE_CURVE('',#1678,#1717,#522,.T.);
#2090=EDGE_CURVE('',#1717,#1718,#260,.T.);
#2091=EDGE_CURVE('',#1718,#1679,#523,.T.);
#2092=EDGE_CURVE('',#1719,#1720,#261,.T.);
#2093=EDGE_CURVE('',#1720,#1681,#524,.T.);
#2094=EDGE_CURVE('',#1680,#1719,#525,.T.);
#2095=EDGE_CURVE('',#1684,#1721,#526,.T.);
#2096=EDGE_CURVE('',#1721,#1722,#262,.T.);
#2097=EDGE_CURVE('',#1722,#1723,#527,.T.);
#2098=EDGE_CURVE('',#1723,#1685,#330,.T.);
#2099=EDGE_CURVE('',#1724,#1725,#263,.T.);
#2100=EDGE_CURVE('',#1725,#1687,#528,.T.);
#2101=EDGE_CURVE('',#1686,#1724,#529,.T.);
#2102=EDGE_CURVE('',#1726,#1727,#264,.T.);
#2103=EDGE_CURVE('',#1727,#1728,#530,.T.);
#2104=EDGE_CURVE('',#1729,#1728,#265,.T.);
#2105=EDGE_CURVE('',#1729,#1730,#331,.T.);
#2106=EDGE_CURVE('',#1730,#1726,#531,.T.);
#2107=EDGE_CURVE('',#1731,#1732,#266,.T.);
#2108=EDGE_CURVE('',#1731,#1733,#532,.T.);
#2109=EDGE_CURVE('',#1733,#1734,#267,.T.);
#2110=EDGE_CURVE('',#1734,#1732,#332,.T.);
#2111=EDGE_CURVE('',#1735,#1736,#333,.T.);
#2112=EDGE_CURVE('',#1736,#1692,#334,.T.);
#2113=EDGE_CURVE('',#1691,#1737,#533,.T.);
#2114=EDGE_CURVE('',#1737,#1735,#1454,.T.);
#2115=EDGE_CURVE('',#1693,#1738,#335,.T.);
#2116=EDGE_CURVE('',#1738,#1739,#336,.T.);
#2117=EDGE_CURVE('',#1739,#1740,#268,.T.);
#2118=EDGE_CURVE('',#1740,#1694,#337,.T.);
#2119=EDGE_CURVE('',#1592,#1696,#338,.T.);
#2120=EDGE_CURVE('',#1695,#1594,#339,.T.);
#2121=EDGE_CURVE('',#1697,#1597,#340,.T.);
#2122=EDGE_CURVE('',#1599,#1698,#341,.T.);
#2123=EDGE_CURVE('',#1600,#1700,#342,.T.);
#2124=EDGE_CURVE('',#1699,#1602,#343,.T.);
#2125=EDGE_CURVE('',#1701,#1605,#344,.T.);
#2126=EDGE_CURVE('',#1607,#1702,#345,.T.);
#2127=EDGE_CURVE('',#1608,#1704,#346,.T.);
#2128=EDGE_CURVE('',#1703,#1610,#347,.T.);
#2129=EDGE_CURVE('',#1705,#1613,#348,.T.);
#2130=EDGE_CURVE('',#1615,#1706,#349,.T.);
#2131=EDGE_CURVE('',#1707,#1741,#534,.T.);
#2132=EDGE_CURVE('',#1741,#1742,#269,.T.);
#2133=EDGE_CURVE('',#1742,#1708,#535,.T.);
#2134=EDGE_CURVE('',#1709,#1617,#1455,.T.);
#2135=EDGE_CURVE('',#1619,#1710,#350,.T.);
#2136=EDGE_CURVE('',#1620,#1712,#351,.T.);
#2137=EDGE_CURVE('',#1711,#1622,#1456,.T.);
#2138=EDGE_CURVE('',#1713,#1625,#1457,.T.);
#2139=EDGE_CURVE('',#1627,#1714,#352,.T.);
#2140=EDGE_CURVE('',#1628,#1716,#353,.T.);
#2141=EDGE_CURVE('',#1715,#1630,#1458,.T.);
#2142=EDGE_CURVE('',#1717,#1633,#1459,.T.);
#2143=EDGE_CURVE('',#1635,#1718,#354,.T.);
#2144=EDGE_CURVE('',#1636,#1720,#355,.T.);
#2145=EDGE_CURVE('',#1719,#1638,#1460,.T.);
#2146=EDGE_CURVE('',#1721,#1641,#1461,.T.);
#2147=EDGE_CURVE('',#1643,#1722,#356,.T.);
#2148=EDGE_CURVE('',#1644,#1725,#357,.T.);
#2149=EDGE_CURVE('',#1724,#1646,#1462,.T.);
#2150=EDGE_CURVE('',#1584,#1727,#358,.T.);
#2151=EDGE_CURVE('',#1726,#1586,#359,.T.);
#2152=EDGE_CURVE('',#1733,#1589,#360,.T.);
#2153=EDGE_CURVE('',#1591,#1734,#361,.T.);
#2154=EDGE_CURVE('',#1667,#1741,#536,.T.);
#2155=EDGE_CURVE('',#1743,#1666,#1463,.T.);
#2156=EDGE_CURVE('',#1742,#1743,#537,.T.);
#2157=EDGE_CURVE('',#1582,#1736,#538,.T.);
#2158=EDGE_CURVE('',#1735,#1744,#1464,.T.);
#2159=EDGE_CURVE('',#1744,#1583,#539,.T.);
#2160=EDGE_CURVE('',#1738,#1579,#540,.T.);
#2161=EDGE_CURVE('',#1578,#1745,#541,.T.);
#2162=EDGE_CURVE('',#1745,#1739,#1465,.T.);
#2163=EDGE_CURVE('',#1665,#1569,#542,.T.);
#2164=EDGE_CURVE('',#1568,#1743,#543,.T.);
#2165=EDGE_CURVE('',#1572,#1621,#544,.T.);
#2166=EDGE_CURVE('',#1623,#1573,#545,.T.);
#2167=EDGE_CURVE('',#1746,#1747,#546,.T.);
#2168=EDGE_CURVE('',#1746,#1748,#270,.T.);
#2169=EDGE_CURVE('',#1749,#1748,#547,.T.);
#2170=EDGE_CURVE('',#1747,#1749,#271,.T.);
#2171=EDGE_CURVE('',#1750,#1751,#548,.T.);
#2172=EDGE_CURVE('',#1752,#1750,#272,.T.);
#2173=EDGE_CURVE('',#1753,#1752,#362,.T.);
#2174=EDGE_CURVE('',#1753,#1751,#273,.T.);
#2175=EDGE_CURVE('',#1682,#1754,#549,.T.);
#2176=EDGE_CURVE('',#1755,#1683,#363,.T.);
#2177=EDGE_CURVE('',#1754,#1755,#274,.T.);
#2178=EDGE_CURVE('',#1756,#1688,#550,.T.);
#2179=EDGE_CURVE('',#1757,#1756,#275,.T.);
#2180=EDGE_CURVE('',#1689,#1757,#364,.T.);
#2181=EDGE_CURVE('',#1728,#1751,#1466,.T.);
#2182=EDGE_CURVE('',#1753,#1729,#365,.T.);
#2183=EDGE_CURVE('',#1758,#1759,#276,.T.);
#2184=EDGE_CURVE('',#1759,#1748,#366,.T.);
#2185=EDGE_CURVE('',#1746,#1731,#367,.T.);
#2186=EDGE_CURVE('',#1732,#1758,#368,.T.);
#2187=EDGE_CURVE('',#1760,#1761,#277,.T.);
#2188=EDGE_CURVE('',#1761,#1762,#551,.T.);
#2189=EDGE_CURVE('',#1762,#1562,#369,.T.);
#2190=EDGE_CURVE('',#1561,#1760,#370,.T.);
#2191=EDGE_CURVE('',#1763,#1764,#371,.T.);
#2192=EDGE_CURVE('',#1764,#1765,#552,.T.);
#2193=EDGE_CURVE('',#1765,#1766,#278,.T.);
#2194=EDGE_CURVE('',#1766,#1767,#372,.T.);
#2195=EDGE_CURVE('',#1763,#1767,#1467,.T.);
#2196=EDGE_CURVE('',#1768,#1769,#279,.T.);
#2197=EDGE_CURVE('',#1769,#1759,#553,.T.);
#2198=EDGE_CURVE('',#1758,#1768,#373,.T.);
#2199=EDGE_CURVE('',#1770,#1771,#280,.T.);
#2200=EDGE_CURVE('',#1771,#1761,#554,.T.);
#2201=EDGE_CURVE('',#1760,#1770,#555,.T.);
#2202=EDGE_CURVE('',#1765,#1772,#556,.T.);
#2203=EDGE_CURVE('',#1772,#1773,#281,.T.);
#2204=EDGE_CURVE('',#1773,#1774,#374,.T.);
#2205=EDGE_CURVE('',#1774,#1766,#1468,.T.);
#2206=EDGE_CURVE('',#1750,#1771,#375,.T.);
#2207=EDGE_CURVE('',#1770,#1754,#1469,.T.);
#2208=EDGE_CURVE('',#1755,#1752,#376,.T.);
#2209=EDGE_CURVE('',#1756,#1769,#377,.T.);
#2210=EDGE_CURVE('',#1768,#1757,#378,.T.);
#2211=EDGE_CURVE('',#1749,#1775,#557,.T.);
#2212=EDGE_CURVE('',#1775,#1773,#379,.T.);
#2213=EDGE_CURVE('',#1772,#1747,#380,.T.);
#2214=EDGE_CURVE('',#1570,#1565,#558,.T.);
#2215=EDGE_CURVE('',#1557,#1564,#559,.T.);
#2216=EDGE_CURVE('',#1774,#1556,#560,.T.);
#2217=EDGE_CURVE('',#1571,#1775,#561,.T.);
#2218=EDGE_CURVE('',#1762,#1581,#562,.T.);
#2219=EDGE_CURVE('',#1764,#1580,#563,.T.);
#2220=EDGE_CURVE('',#1763,#1776,#147,.T.);
#2221=EDGE_CURVE('',#1555,#1776,#564,.T.);
#2222=EDGE_CURVE('',#1563,#1560,#565,.T.);
#2223=EDGE_CURVE('',#1740,#1745,#566,.T.);
#2224=EDGE_CURVE('',#1744,#1737,#567,.T.);
#2225=EDGE_CURVE('',#1567,#1723,#568,.T.);
#2226=EDGE_CURVE('',#1566,#1730,#569,.T.);
#2227=EDGE_CURVE('',#1776,#1767,#1470,.T.);
#2228=EDGE_CURVE('',#1690,#1574,#570,.T.);
#2229=EDGE_CURVE('',#1664,#1577,#571,.T.);
#2230=EDGE_CURVE('',#1777,#1778,#572,.T.);
#2231=EDGE_CURVE('',#1778,#1779,#282,.T.);
#2232=EDGE_CURVE('',#1780,#1779,#1471,.T.);
#2233=EDGE_CURVE('',#1781,#1780,#573,.T.);
#2234=EDGE_CURVE('',#1777,#1781,#283,.T.);
#2235=EDGE_CURVE('',#1782,#1783,#574,.T.);
#2236=EDGE_CURVE('',#1783,#1778,#284,.T.);
#2237=EDGE_CURVE('',#1782,#1777,#285,.T.);
#2238=EDGE_CURVE('',#1784,#1785,#575,.T.);
#2239=EDGE_CURVE('',#1785,#1783,#286,.T.);
#2240=EDGE_CURVE('',#1784,#1782,#287,.T.);
#2241=EDGE_CURVE('',#1786,#1787,#576,.T.);
#2242=EDGE_CURVE('',#1788,#1786,#288,.T.);
#2243=EDGE_CURVE('',#1789,#1788,#577,.T.);
#2244=EDGE_CURVE('',#1789,#1787,#289,.T.);
#2245=EDGE_CURVE('',#1790,#1791,#578,.T.);
#2246=EDGE_CURVE('',#1792,#1791,#1472,.T.);
#2247=EDGE_CURVE('',#1792,#1790,#381,.T.);
#2248=EDGE_CURVE('',#1793,#1794,#579,.T.);
#2249=EDGE_CURVE('',#1795,#1794,#382,.F.);
#2250=EDGE_CURVE('',#1792,#1795,#580,.T.);
#2251=EDGE_CURVE('',#1791,#1792,#1473,.T.);
#2252=EDGE_CURVE('',#1790,#1793,#383,.T.);
#2253=EDGE_CURVE('',#1796,#1797,#581,.T.);
#2254=EDGE_CURVE('',#1794,#1797,#384,.F.);
#2255=EDGE_CURVE('',#1793,#1796,#385,.T.);
#2256=EDGE_CURVE('',#1798,#1799,#582,.T.);
#2257=EDGE_CURVE('',#1798,#1800,#386,.T.);
#2258=EDGE_CURVE('',#1801,#1800,#583,.T.);
#2259=EDGE_CURVE('',#1801,#1802,#1474,.T.);
#2260=EDGE_CURVE('',#1799,#1802,#387,.F.);
#2261=EDGE_CURVE('',#1803,#1803,#1475,.T.);
#2262=EDGE_CURVE('',#1803,#1804,#584,.T.);
#2263=EDGE_CURVE('',#1804,#1804,#1476,.T.);
#2264=EDGE_CURVE('',#1805,#1805,#1477,.T.);
#2265=EDGE_CURVE('',#1805,#1806,#585,.T.);
#2266=EDGE_CURVE('',#1806,#1806,#1478,.T.);
#2267=EDGE_CURVE('',#1807,#1807,#1479,.T.);
#2268=EDGE_CURVE('',#1807,#1808,#586,.T.);
#2269=EDGE_CURVE('',#1808,#1808,#1480,.T.);
#2270=EDGE_CURVE('',#1809,#1809,#1481,.T.);
#2271=EDGE_CURVE('',#1809,#1810,#587,.T.);
#2272=EDGE_CURVE('',#1810,#1810,#1482,.T.);
#2273=EDGE_CURVE('',#1797,#1799,#388,.F.);
#2274=EDGE_CURVE('',#1796,#1798,#389,.T.);
#2275=EDGE_CURVE('',#1801,#1780,#588,.T.);
#2276=EDGE_CURVE('',#1800,#1781,#589,.T.);
#2277=EDGE_CURVE('',#1787,#1785,#290,.T.);
#2278=EDGE_CURVE('',#1786,#1784,#291,.T.);
#2279=EDGE_CURVE('',#1779,#1802,#390,.T.);
#2280=EDGE_CURVE('',#1795,#1789,#590,.T.);
#2281=EDGE_CURVE('',#1788,#1792,#591,.T.);
#2282=EDGE_CURVE('',#1811,#1811,#1483,.T.);
#2283=EDGE_CURVE('',#1811,#1812,#592,.T.);
#2284=EDGE_CURVE('',#1812,#1812,#1484,.T.);
#2285=EDGE_CURVE('',#1813,#1813,#1485,.T.);
#2286=EDGE_CURVE('',#1813,#1814,#593,.T.);
#2287=EDGE_CURVE('',#1814,#1814,#1486,.T.);
#2288=EDGE_CURVE('',#1815,#1815,#1487,.T.);
#2289=EDGE_CURVE('',#1815,#1816,#594,.T.);
#2290=EDGE_CURVE('',#1816,#1816,#1488,.T.);
#2291=EDGE_CURVE('',#1817,#1817,#1489,.T.);
#2292=EDGE_CURVE('',#1817,#1818,#595,.T.);
#2293=EDGE_CURVE('',#1818,#1818,#1490,.T.);
#2294=EDGE_CURVE('',#1819,#1819,#1491,.T.);
#2295=EDGE_CURVE('',#1819,#1820,#596,.T.);
#2296=EDGE_CURVE('',#1820,#1820,#1492,.T.);
#2297=EDGE_CURVE('',#1821,#1821,#1493,.T.);
#2298=EDGE_CURVE('',#1821,#1822,#597,.T.);
#2299=EDGE_CURVE('',#1822,#1822,#1494,.T.);
#2300=EDGE_CURVE('',#1823,#1823,#1495,.T.);
#2301=EDGE_CURVE('',#1823,#1824,#598,.T.);
#2302=EDGE_CURVE('',#1824,#1824,#1496,.T.);
#2303=EDGE_CURVE('',#1825,#1825,#1497,.T.);
#2304=EDGE_CURVE('',#1825,#1826,#599,.T.);
#2305=EDGE_CURVE('',#1826,#1826,#1498,.T.);
#2306=EDGE_CURVE('',#1827,#1827,#1499,.T.);
#2307=EDGE_CURVE('',#1827,#1828,#600,.T.);
#2308=EDGE_CURVE('',#1828,#1828,#1500,.T.);
#2309=EDGE_CURVE('',#1829,#1829,#1501,.T.);
#2310=EDGE_CURVE('',#1829,#1830,#601,.T.);
#2311=EDGE_CURVE('',#1830,#1830,#1502,.T.);
#2312=EDGE_CURVE('',#1831,#1831,#1503,.T.);
#2313=EDGE_CURVE('',#1831,#1832,#602,.T.);
#2314=EDGE_CURVE('',#1832,#1832,#1504,.T.);
#2315=EDGE_CURVE('',#1833,#1833,#1505,.T.);
#2316=EDGE_CURVE('',#1833,#1834,#603,.T.);
#2317=EDGE_CURVE('',#1834,#1834,#1506,.T.);
#2318=EDGE_CURVE('',#1835,#1836,#604,.T.);
#2319=EDGE_CURVE('',#1836,#1837,#605,.T.);
#2320=EDGE_CURVE('',#1837,#1838,#606,.T.);
#2321=EDGE_CURVE('',#1838,#1835,#607,.T.);
#2322=EDGE_CURVE('',#1839,#1840,#608,.T.);
#2323=EDGE_CURVE('',#1840,#1841,#609,.T.);
#2324=EDGE_CURVE('',#1841,#1842,#610,.T.);
#2325=EDGE_CURVE('',#1842,#1839,#611,.T.);
#2326=EDGE_CURVE('',#1843,#1844,#612,.T.);
#2327=EDGE_CURVE('',#1844,#1845,#613,.T.);
#2328=EDGE_CURVE('',#1845,#1846,#614,.T.);
#2329=EDGE_CURVE('',#1846,#1843,#615,.T.);
#2330=EDGE_CURVE('',#1847,#1848,#616,.T.);
#2331=EDGE_CURVE('',#1848,#1849,#617,.T.);
#2332=EDGE_CURVE('',#1849,#1850,#618,.T.);
#2333=EDGE_CURVE('',#1850,#1847,#619,.T.);
#2334=EDGE_CURVE('',#1851,#1852,#620,.T.);
#2335=EDGE_CURVE('',#1852,#1853,#621,.T.);
#2336=EDGE_CURVE('',#1853,#1854,#622,.T.);
#2337=EDGE_CURVE('',#1854,#1851,#623,.T.);
#2338=EDGE_CURVE('',#1855,#1856,#624,.T.);
#2339=EDGE_CURVE('',#1856,#1857,#625,.T.);
#2340=EDGE_CURVE('',#1857,#1858,#626,.T.);
#2341=EDGE_CURVE('',#1858,#1855,#627,.T.);
#2342=EDGE_CURVE('',#1842,#1843,#1507,.T.);
#2343=EDGE_CURVE('',#1844,#1841,#1508,.T.);
#2344=EDGE_CURVE('',#1842,#1851,#1509,.T.);
#2345=EDGE_CURVE('',#1851,#1843,#1510,.T.);
#2346=EDGE_CURVE('',#1844,#1856,#1511,.T.);
#2347=EDGE_CURVE('',#1856,#1841,#1512,.T.);
#2348=EDGE_CURVE('',#1852,#1846,#1513,.T.);
#2349=EDGE_CURVE('',#1839,#1854,#1514,.T.);
#2350=EDGE_CURVE('',#1840,#1837,#1515,.T.);
#2351=EDGE_CURVE('',#1838,#1839,#1516,.T.);
#2352=EDGE_CURVE('',#1857,#1840,#1517,.T.);
#2353=EDGE_CURVE('',#1845,#1855,#1518,.T.);
#2354=EDGE_CURVE('',#1846,#1847,#1519,.T.);
#2355=EDGE_CURVE('',#1848,#1845,#1520,.T.);
#2356=EDGE_CURVE('',#1852,#1847,#1521,.T.);
#2357=EDGE_CURVE('',#1838,#1854,#1522,.T.);
#2358=EDGE_CURVE('',#1857,#1837,#1523,.T.);
#2359=EDGE_CURVE('',#1848,#1855,#1524,.T.);
#2360=EDGE_CURVE('',#1853,#1850,#1525,.T.);
#2361=EDGE_CURVE('',#1835,#1853,#1526,.T.);
#2362=EDGE_CURVE('',#1858,#1836,#1527,.T.);
#2363=EDGE_CURVE('',#1849,#1858,#1528,.T.);
#2364=EDGE_CURVE('',#1835,#1850,#1529,.T.);
#2365=EDGE_CURVE('',#1849,#1836,#1530,.T.);
#2366=EDGE_CURVE('',#1859,#1859,#1531,.T.);
#2367=EDGE_CURVE('',#1859,#1860,#628,.T.);
#2368=EDGE_CURVE('',#1860,#1860,#1532,.T.);
#2369=EDGE_CURVE('',#1861,#1862,#1533,.T.);
#2370=EDGE_CURVE('',#1863,#1861,#292,.T.);
#2371=EDGE_CURVE('',#1864,#1863,#1534,.T.);
#2372=EDGE_CURVE('',#1862,#1864,#293,.T.);
#2373=EDGE_CURVE('',#1865,#1865,#1535,.T.);
#2374=EDGE_CURVE('',#1865,#1866,#629,.T.);
#2375=EDGE_CURVE('',#1867,#1866,#1536,.T.);
#2376=EDGE_CURVE('',#1868,#1867,#630,.T.);
#2377=EDGE_CURVE('',#1861,#1868,#148,.T.);
#2378=EDGE_CURVE('',#1869,#1862,#149,.T.);
#2379=EDGE_CURVE('',#1870,#1869,#631,.T.);
#2380=EDGE_CURVE('',#1866,#1870,#1537,.T.);
#2381=EDGE_CURVE('',#1871,#1872,#1538,.T.);
#2382=EDGE_CURVE('',#1872,#1873,#391,.T.);
#2383=EDGE_CURVE('',#1873,#1874,#1539,.T.);
#2384=EDGE_CURVE('',#1874,#1875,#632,.T.);
#2385=EDGE_CURVE('',#1876,#1875,#1540,.T.);
#2386=EDGE_CURVE('',#1876,#1877,#150,.T.);
#2387=EDGE_CURVE('',#1877,#1878,#633,.T.);
#2388=EDGE_CURVE('',#1878,#1879,#1541,.T.);
#2389=EDGE_CURVE('',#1879,#1880,#634,.T.);
#2390=EDGE_CURVE('',#1880,#1881,#151,.T.);
#2391=EDGE_CURVE('',#1875,#1881,#1542,.T.);
#2392=EDGE_CURVE('',#1874,#1882,#1543,.T.);
#2393=EDGE_CURVE('',#1882,#1871,#392,.T.);
#2394=EDGE_CURVE('',#1873,#1882,#1544,.T.);
#2395=EDGE_CURVE('',#1871,#1872,#1545,.T.);
#2396=EDGE_CURVE('',#1864,#1881,#635,.T.);
#2397=EDGE_CURVE('',#1876,#1863,#636,.T.);
#2398=EDGE_CURVE('',#1879,#1870,#637,.T.);
#2399=EDGE_CURVE('',#1880,#1869,#638,.T.);
#2400=EDGE_CURVE('',#1878,#1867,#639,.T.);
#2401=EDGE_CURVE('',#1877,#1868,#640,.T.);
#2402=ORIENTED_EDGE('',*,*,#1883,.F.);
#2403=ORIENTED_EDGE('',*,*,#1884,.T.);
#2404=ORIENTED_EDGE('',*,*,#1883,.T.);
#2405=ORIENTED_EDGE('',*,*,#1884,.F.);
#2406=ORIENTED_EDGE('',*,*,#1885,.T.);
#2407=ORIENTED_EDGE('',*,*,#1886,.T.);
#2408=ORIENTED_EDGE('',*,*,#1887,.F.);
#2409=ORIENTED_EDGE('',*,*,#1886,.F.);
#2410=ORIENTED_EDGE('',*,*,#1887,.T.);
#2411=ORIENTED_EDGE('',*,*,#1885,.F.);
#2412=ORIENTED_EDGE('',*,*,#1888,.T.);
#2413=ORIENTED_EDGE('',*,*,#1889,.T.);
#2414=ORIENTED_EDGE('',*,*,#1890,.F.);
#2415=ORIENTED_EDGE('',*,*,#1889,.F.);
#2416=ORIENTED_EDGE('',*,*,#1890,.T.);
#2417=ORIENTED_EDGE('',*,*,#1888,.F.);
#2418=ORIENTED_EDGE('',*,*,#1891,.F.);
#2419=ORIENTED_EDGE('',*,*,#1892,.T.);
#2420=ORIENTED_EDGE('',*,*,#1893,.T.);
#2421=ORIENTED_EDGE('',*,*,#1892,.F.);
#2422=ORIENTED_EDGE('',*,*,#1894,.T.);
#2423=ORIENTED_EDGE('',*,*,#1895,.T.);
#2424=ORIENTED_EDGE('',*,*,#1896,.T.);
#2425=ORIENTED_EDGE('',*,*,#1895,.F.);
#2426=ORIENTED_EDGE('',*,*,#1897,.T.);
#2427=ORIENTED_EDGE('',*,*,#1898,.F.);
#2428=ORIENTED_EDGE('',*,*,#1899,.T.);
#2429=ORIENTED_EDGE('',*,*,#1900,.T.);
#2430=ORIENTED_EDGE('',*,*,#1901,.F.);
#2431=ORIENTED_EDGE('',*,*,#1900,.F.);
#2432=ORIENTED_EDGE('',*,*,#1902,.T.);
#2433=ORIENTED_EDGE('',*,*,#1903,.F.);
#2434=ORIENTED_EDGE('',*,*,#1904,.T.);
#2435=ORIENTED_EDGE('',*,*,#1905,.F.);
#2436=ORIENTED_EDGE('',*,*,#1906,.F.);
#2437=ORIENTED_EDGE('',*,*,#1907,.F.);
#2438=ORIENTED_EDGE('',*,*,#1908,.F.);
#2439=ORIENTED_EDGE('',*,*,#1909,.T.);
#2440=ORIENTED_EDGE('',*,*,#1910,.T.);
#2441=ORIENTED_EDGE('',*,*,#1911,.T.);
#2442=ORIENTED_EDGE('',*,*,#1912,.T.);
#2443=ORIENTED_EDGE('',*,*,#1913,.T.);
#2444=ORIENTED_EDGE('',*,*,#1914,.T.);
#2445=ORIENTED_EDGE('',*,*,#1915,.T.);
#2446=ORIENTED_EDGE('',*,*,#1916,.T.);
#2447=ORIENTED_EDGE('',*,*,#1917,.T.);
#2448=ORIENTED_EDGE('',*,*,#1918,.T.);
#2449=ORIENTED_EDGE('',*,*,#1919,.T.);
#2450=ORIENTED_EDGE('',*,*,#1918,.F.);
#2451=ORIENTED_EDGE('',*,*,#1920,.T.);
#2452=ORIENTED_EDGE('',*,*,#1921,.T.);
#2453=ORIENTED_EDGE('',*,*,#1922,.T.);
#2454=ORIENTED_EDGE('',*,*,#1923,.T.);
#2455=ORIENTED_EDGE('',*,*,#1924,.T.);
#2456=ORIENTED_EDGE('',*,*,#1925,.T.);
#2457=ORIENTED_EDGE('',*,*,#1926,.T.);
#2458=ORIENTED_EDGE('',*,*,#1927,.T.);
#2459=ORIENTED_EDGE('',*,*,#1928,.F.);
#2460=ORIENTED_EDGE('',*,*,#1929,.F.);
#2461=ORIENTED_EDGE('',*,*,#1930,.F.);
#2462=ORIENTED_EDGE('',*,*,#1931,.T.);
#2463=ORIENTED_EDGE('',*,*,#1932,.F.);
#2464=ORIENTED_EDGE('',*,*,#1933,.T.);
#2465=ORIENTED_EDGE('',*,*,#1934,.F.);
#2466=ORIENTED_EDGE('',*,*,#1935,.F.);
#2467=ORIENTED_EDGE('',*,*,#1936,.F.);
#2468=ORIENTED_EDGE('',*,*,#1937,.F.);
#2469=ORIENTED_EDGE('',*,*,#1938,.F.);
#2470=ORIENTED_EDGE('',*,*,#1939,.T.);
#2471=ORIENTED_EDGE('',*,*,#1940,.F.);
#2472=ORIENTED_EDGE('',*,*,#1941,.T.);
#2473=ORIENTED_EDGE('',*,*,#1942,.F.);
#2474=ORIENTED_EDGE('',*,*,#1943,.F.);
#2475=ORIENTED_EDGE('',*,*,#1944,.F.);
#2476=ORIENTED_EDGE('',*,*,#1945,.F.);
#2477=ORIENTED_EDGE('',*,*,#1946,.F.);
#2478=ORIENTED_EDGE('',*,*,#1947,.T.);
#2479=ORIENTED_EDGE('',*,*,#1948,.F.);
#2480=ORIENTED_EDGE('',*,*,#1949,.T.);
#2481=ORIENTED_EDGE('',*,*,#1950,.F.);
#2482=ORIENTED_EDGE('',*,*,#1951,.F.);
#2483=ORIENTED_EDGE('',*,*,#1952,.F.);
#2484=ORIENTED_EDGE('',*,*,#1953,.F.);
#2485=ORIENTED_EDGE('',*,*,#1954,.F.);
#2486=ORIENTED_EDGE('',*,*,#1955,.T.);
#2487=ORIENTED_EDGE('',*,*,#1956,.F.);
#2488=ORIENTED_EDGE('',*,*,#1957,.T.);
#2489=ORIENTED_EDGE('',*,*,#1958,.F.);
#2490=ORIENTED_EDGE('',*,*,#1959,.F.);
#2491=ORIENTED_EDGE('',*,*,#1960,.F.);
#2492=ORIENTED_EDGE('',*,*,#1961,.T.);
#2493=ORIENTED_EDGE('',*,*,#1962,.F.);
#2494=ORIENTED_EDGE('',*,*,#1963,.F.);
#2495=ORIENTED_EDGE('',*,*,#1964,.F.);
#2496=ORIENTED_EDGE('',*,*,#1965,.F.);
#2497=ORIENTED_EDGE('',*,*,#1966,.F.);
#2498=ORIENTED_EDGE('',*,*,#1967,.F.);
#2499=ORIENTED_EDGE('',*,*,#1968,.F.);
#2500=ORIENTED_EDGE('',*,*,#1969,.T.);
#2501=ORIENTED_EDGE('',*,*,#1970,.F.);
#2502=ORIENTED_EDGE('',*,*,#1971,.F.);
#2503=ORIENTED_EDGE('',*,*,#1972,.F.);
#2504=ORIENTED_EDGE('',*,*,#1973,.F.);
#2505=ORIENTED_EDGE('',*,*,#1974,.F.);
#2506=ORIENTED_EDGE('',*,*,#1975,.T.);
#2507=ORIENTED_EDGE('',*,*,#1976,.F.);
#2508=ORIENTED_EDGE('',*,*,#1977,.T.);
#2509=ORIENTED_EDGE('',*,*,#1978,.F.);
#2510=ORIENTED_EDGE('',*,*,#1979,.F.);
#2511=ORIENTED_EDGE('',*,*,#1980,.F.);
#2512=ORIENTED_EDGE('',*,*,#1981,.F.);
#2513=ORIENTED_EDGE('',*,*,#1982,.F.);
#2514=ORIENTED_EDGE('',*,*,#1983,.T.);
#2515=ORIENTED_EDGE('',*,*,#1984,.F.);
#2516=ORIENTED_EDGE('',*,*,#1985,.T.);
#2517=ORIENTED_EDGE('',*,*,#1986,.F.);
#2518=ORIENTED_EDGE('',*,*,#1987,.F.);
#2519=ORIENTED_EDGE('',*,*,#1988,.F.);
#2520=ORIENTED_EDGE('',*,*,#1989,.F.);
#2521=ORIENTED_EDGE('',*,*,#1990,.F.);
#2522=ORIENTED_EDGE('',*,*,#1991,.T.);
#2523=ORIENTED_EDGE('',*,*,#1992,.T.);
#2524=ORIENTED_EDGE('',*,*,#1993,.T.);
#2525=ORIENTED_EDGE('',*,*,#1939,.F.);
#2526=ORIENTED_EDGE('',*,*,#1994,.T.);
#2527=ORIENTED_EDGE('',*,*,#1941,.F.);
#2528=ORIENTED_EDGE('',*,*,#1995,.T.);
#2529=ORIENTED_EDGE('',*,*,#1996,.T.);
#2530=ORIENTED_EDGE('',*,*,#1997,.T.);
#2531=ORIENTED_EDGE('',*,*,#1998,.T.);
#2532=ORIENTED_EDGE('',*,*,#1999,.T.);
#2533=ORIENTED_EDGE('',*,*,#1947,.F.);
#2534=ORIENTED_EDGE('',*,*,#2000,.T.);
#2535=ORIENTED_EDGE('',*,*,#1949,.F.);
#2536=ORIENTED_EDGE('',*,*,#2001,.T.);
#2537=ORIENTED_EDGE('',*,*,#2002,.T.);
#2538=ORIENTED_EDGE('',*,*,#2003,.T.);
#2539=ORIENTED_EDGE('',*,*,#2004,.T.);
#2540=ORIENTED_EDGE('',*,*,#2005,.T.);
#2541=ORIENTED_EDGE('',*,*,#1955,.F.);
#2542=ORIENTED_EDGE('',*,*,#2006,.T.);
#2543=ORIENTED_EDGE('',*,*,#1957,.F.);
#2544=ORIENTED_EDGE('',*,*,#2007,.T.);
#2545=ORIENTED_EDGE('',*,*,#2008,.T.);
#2546=ORIENTED_EDGE('',*,*,#2009,.T.);
#2547=ORIENTED_EDGE('',*,*,#2010,.T.);
#2548=ORIENTED_EDGE('',*,*,#2011,.T.);
#2549=ORIENTED_EDGE('',*,*,#1931,.F.);
#2550=ORIENTED_EDGE('',*,*,#2012,.T.);
#2551=ORIENTED_EDGE('',*,*,#1933,.F.);
#2552=ORIENTED_EDGE('',*,*,#2013,.T.);
#2553=ORIENTED_EDGE('',*,*,#2014,.T.);
#2554=ORIENTED_EDGE('',*,*,#2015,.T.);
#2555=ORIENTED_EDGE('',*,*,#2016,.T.);
#2556=ORIENTED_EDGE('',*,*,#1961,.F.);
#2557=ORIENTED_EDGE('',*,*,#2017,.T.);
#2558=ORIENTED_EDGE('',*,*,#2018,.T.);
#2559=ORIENTED_EDGE('',*,*,#2019,.T.);
#2560=ORIENTED_EDGE('',*,*,#2020,.T.);
#2561=ORIENTED_EDGE('',*,*,#2021,.T.);
#2562=ORIENTED_EDGE('',*,*,#2022,.T.);
#2563=ORIENTED_EDGE('',*,*,#1969,.F.);
#2564=ORIENTED_EDGE('',*,*,#2023,.T.);
#2565=ORIENTED_EDGE('',*,*,#2024,.T.);
#2566=ORIENTED_EDGE('',*,*,#2025,.T.);
#2567=ORIENTED_EDGE('',*,*,#2026,.T.);
#2568=ORIENTED_EDGE('',*,*,#2027,.T.);
#2569=ORIENTED_EDGE('',*,*,#1975,.F.);
#2570=ORIENTED_EDGE('',*,*,#2028,.T.);
#2571=ORIENTED_EDGE('',*,*,#1977,.F.);
#2572=ORIENTED_EDGE('',*,*,#2029,.T.);
#2573=ORIENTED_EDGE('',*,*,#2030,.T.);
#2574=ORIENTED_EDGE('',*,*,#2031,.T.);
#2575=ORIENTED_EDGE('',*,*,#2032,.T.);
#2576=ORIENTED_EDGE('',*,*,#2033,.T.);
#2577=ORIENTED_EDGE('',*,*,#1983,.F.);
#2578=ORIENTED_EDGE('',*,*,#2034,.T.);
#2579=ORIENTED_EDGE('',*,*,#1985,.F.);
#2580=ORIENTED_EDGE('',*,*,#2035,.T.);
#2581=ORIENTED_EDGE('',*,*,#2036,.T.);
#2582=ORIENTED_EDGE('',*,*,#2037,.T.);
#2583=ORIENTED_EDGE('',*,*,#2038,.T.);
#2584=ORIENTED_EDGE('',*,*,#2039,.T.);
#2585=ORIENTED_EDGE('',*,*,#1991,.F.);
#2586=ORIENTED_EDGE('',*,*,#2040,.T.);
#2587=ORIENTED_EDGE('',*,*,#2041,.F.);
#2588=ORIENTED_EDGE('',*,*,#2042,.T.);
#2589=ORIENTED_EDGE('',*,*,#2043,.T.);
#2590=ORIENTED_EDGE('',*,*,#2044,.T.);
#2591=ORIENTED_EDGE('',*,*,#2045,.T.);
#2592=ORIENTED_EDGE('',*,*,#2046,.T.);
#2593=ORIENTED_EDGE('',*,*,#2047,.F.);
#2594=ORIENTED_EDGE('',*,*,#2048,.T.);
#2595=ORIENTED_EDGE('',*,*,#2049,.T.);
#2596=ORIENTED_EDGE('',*,*,#2050,.T.);
#2597=ORIENTED_EDGE('',*,*,#2051,.T.);
#2598=ORIENTED_EDGE('',*,*,#1992,.F.);
#2599=ORIENTED_EDGE('',*,*,#2052,.T.);
#2600=ORIENTED_EDGE('',*,*,#1996,.F.);
#2601=ORIENTED_EDGE('',*,*,#2053,.T.);
#2602=ORIENTED_EDGE('',*,*,#2054,.T.);
#2603=ORIENTED_EDGE('',*,*,#2055,.T.);
#2604=ORIENTED_EDGE('',*,*,#2056,.T.);
#2605=ORIENTED_EDGE('',*,*,#2057,.T.);
#2606=ORIENTED_EDGE('',*,*,#1998,.F.);
#2607=ORIENTED_EDGE('',*,*,#2058,.T.);
#2608=ORIENTED_EDGE('',*,*,#2002,.F.);
#2609=ORIENTED_EDGE('',*,*,#2059,.T.);
#2610=ORIENTED_EDGE('',*,*,#2060,.T.);
#2611=ORIENTED_EDGE('',*,*,#2061,.T.);
#2612=ORIENTED_EDGE('',*,*,#2062,.T.);
#2613=ORIENTED_EDGE('',*,*,#2063,.T.);
#2614=ORIENTED_EDGE('',*,*,#2004,.F.);
#2615=ORIENTED_EDGE('',*,*,#2064,.T.);
#2616=ORIENTED_EDGE('',*,*,#2008,.F.);
#2617=ORIENTED_EDGE('',*,*,#2065,.T.);
#2618=ORIENTED_EDGE('',*,*,#2066,.T.);
#2619=ORIENTED_EDGE('',*,*,#2067,.T.);
#2620=ORIENTED_EDGE('',*,*,#2068,.T.);
#2621=ORIENTED_EDGE('',*,*,#2069,.T.);
#2622=ORIENTED_EDGE('',*,*,#2010,.F.);
#2623=ORIENTED_EDGE('',*,*,#2070,.T.);
#2624=ORIENTED_EDGE('',*,*,#2014,.F.);
#2625=ORIENTED_EDGE('',*,*,#2071,.T.);
#2626=ORIENTED_EDGE('',*,*,#2072,.T.);
#2627=ORIENTED_EDGE('',*,*,#2073,.T.);
#2628=ORIENTED_EDGE('',*,*,#2021,.F.);
#2629=ORIENTED_EDGE('',*,*,#2074,.T.);
#2630=ORIENTED_EDGE('',*,*,#2075,.T.);
#2631=ORIENTED_EDGE('',*,*,#2076,.T.);
#2632=ORIENTED_EDGE('',*,*,#2024,.F.);
#2633=ORIENTED_EDGE('',*,*,#2077,.T.);
#2634=ORIENTED_EDGE('',*,*,#2078,.T.);
#2635=ORIENTED_EDGE('',*,*,#2079,.T.);
#2636=ORIENTED_EDGE('',*,*,#2080,.T.);
#2637=ORIENTED_EDGE('',*,*,#2081,.T.);
#2638=ORIENTED_EDGE('',*,*,#2026,.F.);
#2639=ORIENTED_EDGE('',*,*,#2082,.T.);
#2640=ORIENTED_EDGE('',*,*,#2030,.F.);
#2641=ORIENTED_EDGE('',*,*,#2083,.T.);
#2642=ORIENTED_EDGE('',*,*,#2084,.T.);
#2643=ORIENTED_EDGE('',*,*,#2085,.T.);
#2644=ORIENTED_EDGE('',*,*,#2086,.T.);
#2645=ORIENTED_EDGE('',*,*,#2087,.T.);
#2646=ORIENTED_EDGE('',*,*,#2032,.F.);
#2647=ORIENTED_EDGE('',*,*,#2088,.T.);
#2648=ORIENTED_EDGE('',*,*,#2036,.F.);
#2649=ORIENTED_EDGE('',*,*,#2089,.T.);
#2650=ORIENTED_EDGE('',*,*,#2090,.T.);
#2651=ORIENTED_EDGE('',*,*,#2091,.T.);
#2652=ORIENTED_EDGE('',*,*,#2092,.T.);
#2653=ORIENTED_EDGE('',*,*,#2093,.T.);
#2654=ORIENTED_EDGE('',*,*,#2038,.F.);
#2655=ORIENTED_EDGE('',*,*,#2094,.T.);
#2656=ORIENTED_EDGE('',*,*,#2043,.F.);
#2657=ORIENTED_EDGE('',*,*,#2095,.T.);
#2658=ORIENTED_EDGE('',*,*,#2096,.T.);
#2659=ORIENTED_EDGE('',*,*,#2097,.T.);
#2660=ORIENTED_EDGE('',*,*,#2098,.T.);
#2661=ORIENTED_EDGE('',*,*,#2099,.T.);
#2662=ORIENTED_EDGE('',*,*,#2100,.T.);
#2663=ORIENTED_EDGE('',*,*,#2045,.F.);
#2664=ORIENTED_EDGE('',*,*,#2101,.T.);
#2665=ORIENTED_EDGE('',*,*,#2102,.T.);
#2666=ORIENTED_EDGE('',*,*,#2103,.T.);
#2667=ORIENTED_EDGE('',*,*,#2104,.F.);
#2668=ORIENTED_EDGE('',*,*,#2105,.T.);
#2669=ORIENTED_EDGE('',*,*,#2106,.T.);
#2670=ORIENTED_EDGE('',*,*,#2107,.F.);
#2671=ORIENTED_EDGE('',*,*,#2108,.T.);
#2672=ORIENTED_EDGE('',*,*,#2109,.T.);
#2673=ORIENTED_EDGE('',*,*,#2110,.T.);
#2674=ORIENTED_EDGE('',*,*,#2111,.T.);
#2675=ORIENTED_EDGE('',*,*,#2112,.T.);
#2676=ORIENTED_EDGE('',*,*,#2050,.F.);
#2677=ORIENTED_EDGE('',*,*,#2113,.T.);
#2678=ORIENTED_EDGE('',*,*,#2114,.T.);
#2679=ORIENTED_EDGE('',*,*,#2054,.F.);
#2680=ORIENTED_EDGE('',*,*,#2115,.T.);
#2681=ORIENTED_EDGE('',*,*,#2116,.T.);
#2682=ORIENTED_EDGE('',*,*,#2117,.T.);
#2683=ORIENTED_EDGE('',*,*,#2118,.T.);
#2684=ORIENTED_EDGE('',*,*,#1937,.T.);
#2685=ORIENTED_EDGE('',*,*,#2119,.T.);
#2686=ORIENTED_EDGE('',*,*,#2056,.F.);
#2687=ORIENTED_EDGE('',*,*,#2120,.T.);
#2688=ORIENTED_EDGE('',*,*,#2060,.F.);
#2689=ORIENTED_EDGE('',*,*,#2121,.T.);
#2690=ORIENTED_EDGE('',*,*,#1943,.T.);
#2691=ORIENTED_EDGE('',*,*,#2122,.T.);
#2692=ORIENTED_EDGE('',*,*,#1945,.T.);
#2693=ORIENTED_EDGE('',*,*,#2123,.T.);
#2694=ORIENTED_EDGE('',*,*,#2062,.F.);
#2695=ORIENTED_EDGE('',*,*,#2124,.T.);
#2696=ORIENTED_EDGE('',*,*,#2066,.F.);
#2697=ORIENTED_EDGE('',*,*,#2125,.T.);
#2698=ORIENTED_EDGE('',*,*,#1951,.T.);
#2699=ORIENTED_EDGE('',*,*,#2126,.T.);
#2700=ORIENTED_EDGE('',*,*,#1953,.T.);
#2701=ORIENTED_EDGE('',*,*,#2127,.T.);
#2702=ORIENTED_EDGE('',*,*,#2068,.F.);
#2703=ORIENTED_EDGE('',*,*,#2128,.T.);
#2704=ORIENTED_EDGE('',*,*,#2072,.F.);
#2705=ORIENTED_EDGE('',*,*,#2129,.T.);
#2706=ORIENTED_EDGE('',*,*,#1959,.T.);
#2707=ORIENTED_EDGE('',*,*,#2130,.T.);
#2708=ORIENTED_EDGE('',*,*,#2075,.F.);
#2709=ORIENTED_EDGE('',*,*,#2131,.T.);
#2710=ORIENTED_EDGE('',*,*,#2132,.T.);
#2711=ORIENTED_EDGE('',*,*,#2133,.T.);
#2712=ORIENTED_EDGE('',*,*,#2078,.F.);
#2713=ORIENTED_EDGE('',*,*,#2134,.T.);
#2714=ORIENTED_EDGE('',*,*,#1963,.T.);
#2715=ORIENTED_EDGE('',*,*,#2135,.T.);
#2716=ORIENTED_EDGE('',*,*,#1965,.T.);
#2717=ORIENTED_EDGE('',*,*,#2136,.T.);
#2718=ORIENTED_EDGE('',*,*,#2080,.F.);
#2719=ORIENTED_EDGE('',*,*,#2137,.T.);
#2720=ORIENTED_EDGE('',*,*,#2084,.F.);
#2721=ORIENTED_EDGE('',*,*,#2138,.T.);
#2722=ORIENTED_EDGE('',*,*,#1971,.T.);
#2723=ORIENTED_EDGE('',*,*,#2139,.T.);
#2724=ORIENTED_EDGE('',*,*,#1973,.T.);
#2725=ORIENTED_EDGE('',*,*,#2140,.T.);
#2726=ORIENTED_EDGE('',*,*,#2086,.F.);
#2727=ORIENTED_EDGE('',*,*,#2141,.T.);
#2728=ORIENTED_EDGE('',*,*,#2090,.F.);
#2729=ORIENTED_EDGE('',*,*,#2142,.T.);
#2730=ORIENTED_EDGE('',*,*,#1979,.T.);
#2731=ORIENTED_EDGE('',*,*,#2143,.T.);
#2732=ORIENTED_EDGE('',*,*,#1981,.T.);
#2733=ORIENTED_EDGE('',*,*,#2144,.T.);
#2734=ORIENTED_EDGE('',*,*,#2092,.F.);
#2735=ORIENTED_EDGE('',*,*,#2145,.T.);
#2736=ORIENTED_EDGE('',*,*,#2096,.F.);
#2737=ORIENTED_EDGE('',*,*,#2146,.T.);
#2738=ORIENTED_EDGE('',*,*,#1987,.T.);
#2739=ORIENTED_EDGE('',*,*,#2147,.T.);
#2740=ORIENTED_EDGE('',*,*,#1989,.T.);
#2741=ORIENTED_EDGE('',*,*,#2148,.T.);
#2742=ORIENTED_EDGE('',*,*,#2099,.F.);
#2743=ORIENTED_EDGE('',*,*,#2149,.T.);
#2744=ORIENTED_EDGE('',*,*,#1929,.T.);
#2745=ORIENTED_EDGE('',*,*,#2150,.T.);
#2746=ORIENTED_EDGE('',*,*,#2102,.F.);
#2747=ORIENTED_EDGE('',*,*,#2151,.T.);
#2748=ORIENTED_EDGE('',*,*,#2109,.F.);
#2749=ORIENTED_EDGE('',*,*,#2152,.T.);
#2750=ORIENTED_EDGE('',*,*,#1935,.T.);
#2751=ORIENTED_EDGE('',*,*,#2153,.T.);
#2752=ORIENTED_EDGE('',*,*,#2154,.F.);
#2753=ORIENTED_EDGE('',*,*,#2019,.F.);
#2754=ORIENTED_EDGE('',*,*,#2155,.F.);
#2755=ORIENTED_EDGE('',*,*,#2156,.F.);
#2756=ORIENTED_EDGE('',*,*,#2132,.F.);
#2757=ORIENTED_EDGE('',*,*,#1926,.F.);
#2758=ORIENTED_EDGE('',*,*,#2157,.T.);
#2759=ORIENTED_EDGE('',*,*,#2111,.F.);
#2760=ORIENTED_EDGE('',*,*,#2158,.T.);
#2761=ORIENTED_EDGE('',*,*,#2159,.T.);
#2762=ORIENTED_EDGE('',*,*,#2116,.F.);
#2763=ORIENTED_EDGE('',*,*,#2160,.T.);
#2764=ORIENTED_EDGE('',*,*,#1922,.F.);
#2765=ORIENTED_EDGE('',*,*,#2161,.T.);
#2766=ORIENTED_EDGE('',*,*,#2162,.T.);
#2767=ORIENTED_EDGE('',*,*,#2018,.F.);
#2768=ORIENTED_EDGE('',*,*,#2163,.T.);
#2769=ORIENTED_EDGE('',*,*,#1911,.F.);
#2770=ORIENTED_EDGE('',*,*,#2164,.T.);
#2771=ORIENTED_EDGE('',*,*,#2155,.T.);
#2772=ORIENTED_EDGE('',*,*,#1915,.F.);
#2773=ORIENTED_EDGE('',*,*,#2165,.T.);
#2774=ORIENTED_EDGE('',*,*,#1967,.T.);
#2775=ORIENTED_EDGE('',*,*,#2166,.T.);
#2776=ORIENTED_EDGE('',*,*,#2167,.F.);
#2777=ORIENTED_EDGE('',*,*,#2168,.T.);
#2778=ORIENTED_EDGE('',*,*,#2169,.F.);
#2779=ORIENTED_EDGE('',*,*,#2170,.F.);
#2780=ORIENTED_EDGE('',*,*,#2171,.F.);
#2781=ORIENTED_EDGE('',*,*,#2172,.F.);
#2782=ORIENTED_EDGE('',*,*,#2173,.F.);
#2783=ORIENTED_EDGE('',*,*,#2174,.T.);
#2784=ORIENTED_EDGE('',*,*,#2175,.F.);
#2785=ORIENTED_EDGE('',*,*,#2041,.T.);
#2786=ORIENTED_EDGE('',*,*,#2176,.F.);
#2787=ORIENTED_EDGE('',*,*,#2177,.F.);
#2788=ORIENTED_EDGE('',*,*,#2178,.F.);
#2789=ORIENTED_EDGE('',*,*,#2179,.F.);
#2790=ORIENTED_EDGE('',*,*,#2180,.F.);
#2791=ORIENTED_EDGE('',*,*,#2047,.T.);
#2792=ORIENTED_EDGE('',*,*,#2104,.T.);
#2793=ORIENTED_EDGE('',*,*,#2181,.T.);
#2794=ORIENTED_EDGE('',*,*,#2174,.F.);
#2795=ORIENTED_EDGE('',*,*,#2182,.T.);
#2796=ORIENTED_EDGE('',*,*,#2183,.T.);
#2797=ORIENTED_EDGE('',*,*,#2184,.T.);
#2798=ORIENTED_EDGE('',*,*,#2168,.F.);
#2799=ORIENTED_EDGE('',*,*,#2185,.T.);
#2800=ORIENTED_EDGE('',*,*,#2107,.T.);
#2801=ORIENTED_EDGE('',*,*,#2186,.T.);
#2802=ORIENTED_EDGE('',*,*,#2187,.T.);
#2803=ORIENTED_EDGE('',*,*,#2188,.T.);
#2804=ORIENTED_EDGE('',*,*,#2189,.T.);
#2805=ORIENTED_EDGE('',*,*,#1904,.F.);
#2806=ORIENTED_EDGE('',*,*,#2190,.T.);
#2807=ORIENTED_EDGE('',*,*,#2191,.T.);
#2808=ORIENTED_EDGE('',*,*,#2192,.T.);
#2809=ORIENTED_EDGE('',*,*,#2193,.T.);
#2810=ORIENTED_EDGE('',*,*,#2194,.T.);
#2811=ORIENTED_EDGE('',*,*,#2195,.F.);
#2812=ORIENTED_EDGE('',*,*,#2196,.T.);
#2813=ORIENTED_EDGE('',*,*,#2197,.T.);
#2814=ORIENTED_EDGE('',*,*,#2183,.F.);
#2815=ORIENTED_EDGE('',*,*,#2198,.T.);
#2816=ORIENTED_EDGE('',*,*,#2199,.T.);
#2817=ORIENTED_EDGE('',*,*,#2200,.T.);
#2818=ORIENTED_EDGE('',*,*,#2187,.F.);
#2819=ORIENTED_EDGE('',*,*,#2201,.T.);
#2820=ORIENTED_EDGE('',*,*,#2193,.F.);
#2821=ORIENTED_EDGE('',*,*,#2202,.T.);
#2822=ORIENTED_EDGE('',*,*,#2203,.T.);
#2823=ORIENTED_EDGE('',*,*,#2204,.T.);
#2824=ORIENTED_EDGE('',*,*,#2205,.T.);
#2825=ORIENTED_EDGE('',*,*,#2172,.T.);
#2826=ORIENTED_EDGE('',*,*,#2206,.T.);
#2827=ORIENTED_EDGE('',*,*,#2199,.F.);
#2828=ORIENTED_EDGE('',*,*,#2207,.T.);
#2829=ORIENTED_EDGE('',*,*,#2177,.T.);
#2830=ORIENTED_EDGE('',*,*,#2208,.T.);
#2831=ORIENTED_EDGE('',*,*,#2179,.T.);
#2832=ORIENTED_EDGE('',*,*,#2209,.T.);
#2833=ORIENTED_EDGE('',*,*,#2196,.F.);
#2834=ORIENTED_EDGE('',*,*,#2210,.T.);
#2835=ORIENTED_EDGE('',*,*,#2170,.T.);
#2836=ORIENTED_EDGE('',*,*,#2211,.T.);
#2837=ORIENTED_EDGE('',*,*,#2212,.T.);
#2838=ORIENTED_EDGE('',*,*,#2203,.F.);
#2839=ORIENTED_EDGE('',*,*,#2213,.T.);
#2840=ORIENTED_EDGE('',*,*,#1913,.F.);
#2841=ORIENTED_EDGE('',*,*,#2214,.T.);
#2842=ORIENTED_EDGE('',*,*,#1907,.T.);
#2843=ORIENTED_EDGE('',*,*,#2215,.F.);
#2844=ORIENTED_EDGE('',*,*,#1898,.T.);
#2845=ORIENTED_EDGE('',*,*,#2216,.F.);
#2846=ORIENTED_EDGE('',*,*,#2204,.F.);
#2847=ORIENTED_EDGE('',*,*,#2212,.F.);
#2848=ORIENTED_EDGE('',*,*,#2217,.F.);
#2849=ORIENTED_EDGE('',*,*,#2189,.F.);
#2850=ORIENTED_EDGE('',*,*,#2218,.T.);
#2851=ORIENTED_EDGE('',*,*,#1924,.F.);
#2852=ORIENTED_EDGE('',*,*,#2219,.F.);
#2853=ORIENTED_EDGE('',*,*,#2191,.F.);
#2854=ORIENTED_EDGE('',*,*,#2220,.T.);
#2855=ORIENTED_EDGE('',*,*,#2221,.F.);
#2856=ORIENTED_EDGE('',*,*,#1903,.T.);
#2857=ORIENTED_EDGE('',*,*,#2222,.F.);
#2858=ORIENTED_EDGE('',*,*,#1905,.T.);
#2859=ORIENTED_EDGE('',*,*,#2223,.F.);
#2860=ORIENTED_EDGE('',*,*,#2117,.F.);
#2861=ORIENTED_EDGE('',*,*,#2162,.F.);
#2862=ORIENTED_EDGE('',*,*,#2224,.F.);
#2863=ORIENTED_EDGE('',*,*,#2158,.F.);
#2864=ORIENTED_EDGE('',*,*,#2114,.F.);
#2865=ORIENTED_EDGE('',*,*,#2225,.F.);
#2866=ORIENTED_EDGE('',*,*,#1909,.F.);
#2867=ORIENTED_EDGE('',*,*,#2226,.T.);
#2868=ORIENTED_EDGE('',*,*,#2105,.F.);
#2869=ORIENTED_EDGE('',*,*,#2182,.F.);
#2870=ORIENTED_EDGE('',*,*,#2173,.T.);
#2871=ORIENTED_EDGE('',*,*,#2208,.F.);
#2872=ORIENTED_EDGE('',*,*,#2176,.T.);
#2873=ORIENTED_EDGE('',*,*,#2044,.F.);
#2874=ORIENTED_EDGE('',*,*,#2098,.F.);
#2875=ORIENTED_EDGE('',*,*,#2220,.F.);
#2876=ORIENTED_EDGE('',*,*,#2195,.T.);
#2877=ORIENTED_EDGE('',*,*,#2227,.F.);
#2878=ORIENTED_EDGE('',*,*,#2205,.F.);
#2879=ORIENTED_EDGE('',*,*,#2216,.T.);
#2880=ORIENTED_EDGE('',*,*,#1897,.F.);
#2881=ORIENTED_EDGE('',*,*,#2221,.T.);
#2882=ORIENTED_EDGE('',*,*,#2227,.T.);
#2883=ORIENTED_EDGE('',*,*,#2194,.F.);
#2884=ORIENTED_EDGE('',*,*,#1906,.T.);
#2885=ORIENTED_EDGE('',*,*,#2222,.T.);
#2886=ORIENTED_EDGE('',*,*,#1902,.F.);
#2887=ORIENTED_EDGE('',*,*,#1899,.F.);
#2888=ORIENTED_EDGE('',*,*,#2215,.T.);
#2889=ORIENTED_EDGE('',*,*,#1894,.F.);
#2890=ORIENTED_EDGE('',*,*,#1893,.F.);
#2891=ORIENTED_EDGE('',*,*,#1896,.F.);
#2892=ORIENTED_EDGE('',*,*,#1901,.T.);
#2893=ORIENTED_EDGE('',*,*,#2228,.F.);
#2894=ORIENTED_EDGE('',*,*,#2048,.F.);
#2895=ORIENTED_EDGE('',*,*,#2180,.T.);
#2896=ORIENTED_EDGE('',*,*,#2210,.F.);
#2897=ORIENTED_EDGE('',*,*,#2198,.F.);
#2898=ORIENTED_EDGE('',*,*,#2186,.F.);
#2899=ORIENTED_EDGE('',*,*,#2110,.F.);
#2900=ORIENTED_EDGE('',*,*,#2153,.F.);
#2901=ORIENTED_EDGE('',*,*,#1934,.T.);
#2902=ORIENTED_EDGE('',*,*,#2016,.F.);
#2903=ORIENTED_EDGE('',*,*,#2229,.T.);
#2904=ORIENTED_EDGE('',*,*,#1920,.F.);
#2905=ORIENTED_EDGE('',*,*,#1917,.F.);
#2906=ORIENTED_EDGE('',*,*,#2147,.F.);
#2907=ORIENTED_EDGE('',*,*,#1986,.T.);
#2908=ORIENTED_EDGE('',*,*,#2037,.F.);
#2909=ORIENTED_EDGE('',*,*,#2091,.F.);
#2910=ORIENTED_EDGE('',*,*,#2143,.F.);
#2911=ORIENTED_EDGE('',*,*,#1978,.T.);
#2912=ORIENTED_EDGE('',*,*,#2031,.F.);
#2913=ORIENTED_EDGE('',*,*,#2085,.F.);
#2914=ORIENTED_EDGE('',*,*,#2139,.F.);
#2915=ORIENTED_EDGE('',*,*,#1970,.T.);
#2916=ORIENTED_EDGE('',*,*,#2025,.F.);
#2917=ORIENTED_EDGE('',*,*,#2079,.F.);
#2918=ORIENTED_EDGE('',*,*,#2135,.F.);
#2919=ORIENTED_EDGE('',*,*,#1962,.T.);
#2920=ORIENTED_EDGE('',*,*,#2022,.F.);
#2921=ORIENTED_EDGE('',*,*,#2076,.F.);
#2922=ORIENTED_EDGE('',*,*,#2133,.F.);
#2923=ORIENTED_EDGE('',*,*,#2156,.T.);
#2924=ORIENTED_EDGE('',*,*,#2164,.F.);
#2925=ORIENTED_EDGE('',*,*,#1910,.F.);
#2926=ORIENTED_EDGE('',*,*,#2225,.T.);
#2927=ORIENTED_EDGE('',*,*,#2097,.F.);
#2928=ORIENTED_EDGE('',*,*,#2159,.F.);
#2929=ORIENTED_EDGE('',*,*,#2224,.T.);
#2930=ORIENTED_EDGE('',*,*,#2113,.F.);
#2931=ORIENTED_EDGE('',*,*,#2052,.F.);
#2932=ORIENTED_EDGE('',*,*,#1994,.F.);
#2933=ORIENTED_EDGE('',*,*,#1938,.T.);
#2934=ORIENTED_EDGE('',*,*,#2120,.F.);
#2935=ORIENTED_EDGE('',*,*,#2058,.F.);
#2936=ORIENTED_EDGE('',*,*,#2000,.F.);
#2937=ORIENTED_EDGE('',*,*,#1946,.T.);
#2938=ORIENTED_EDGE('',*,*,#2124,.F.);
#2939=ORIENTED_EDGE('',*,*,#2064,.F.);
#2940=ORIENTED_EDGE('',*,*,#2006,.F.);
#2941=ORIENTED_EDGE('',*,*,#1954,.T.);
#2942=ORIENTED_EDGE('',*,*,#2128,.F.);
#2943=ORIENTED_EDGE('',*,*,#2070,.F.);
#2944=ORIENTED_EDGE('',*,*,#2012,.F.);
#2945=ORIENTED_EDGE('',*,*,#1930,.T.);
#2946=ORIENTED_EDGE('',*,*,#2151,.F.);
#2947=ORIENTED_EDGE('',*,*,#2106,.F.);
#2948=ORIENTED_EDGE('',*,*,#2226,.F.);
#2949=ORIENTED_EDGE('',*,*,#1927,.F.);
#2950=ORIENTED_EDGE('',*,*,#2228,.T.);
#2951=ORIENTED_EDGE('',*,*,#1916,.F.);
#2952=ORIENTED_EDGE('',*,*,#2166,.F.);
#2953=ORIENTED_EDGE('',*,*,#1966,.T.);
#2954=ORIENTED_EDGE('',*,*,#2137,.F.);
#2955=ORIENTED_EDGE('',*,*,#2082,.F.);
#2956=ORIENTED_EDGE('',*,*,#2028,.F.);
#2957=ORIENTED_EDGE('',*,*,#1974,.T.);
#2958=ORIENTED_EDGE('',*,*,#2141,.F.);
#2959=ORIENTED_EDGE('',*,*,#2088,.F.);
#2960=ORIENTED_EDGE('',*,*,#2034,.F.);
#2961=ORIENTED_EDGE('',*,*,#1982,.T.);
#2962=ORIENTED_EDGE('',*,*,#2145,.F.);
#2963=ORIENTED_EDGE('',*,*,#2094,.F.);
#2964=ORIENTED_EDGE('',*,*,#2040,.F.);
#2965=ORIENTED_EDGE('',*,*,#1990,.T.);
#2966=ORIENTED_EDGE('',*,*,#2149,.F.);
#2967=ORIENTED_EDGE('',*,*,#2101,.F.);
#2968=ORIENTED_EDGE('',*,*,#2049,.F.);
#2969=ORIENTED_EDGE('',*,*,#2126,.F.);
#2970=ORIENTED_EDGE('',*,*,#1950,.T.);
#2971=ORIENTED_EDGE('',*,*,#2003,.F.);
#2972=ORIENTED_EDGE('',*,*,#2061,.F.);
#2973=ORIENTED_EDGE('',*,*,#2122,.F.);
#2974=ORIENTED_EDGE('',*,*,#1942,.T.);
#2975=ORIENTED_EDGE('',*,*,#1997,.F.);
#2976=ORIENTED_EDGE('',*,*,#2055,.F.);
#2977=ORIENTED_EDGE('',*,*,#2118,.F.);
#2978=ORIENTED_EDGE('',*,*,#2223,.T.);
#2979=ORIENTED_EDGE('',*,*,#2161,.F.);
#2980=ORIENTED_EDGE('',*,*,#1921,.F.);
#2981=ORIENTED_EDGE('',*,*,#2229,.F.);
#2982=ORIENTED_EDGE('',*,*,#2015,.F.);
#2983=ORIENTED_EDGE('',*,*,#2073,.F.);
#2984=ORIENTED_EDGE('',*,*,#2130,.F.);
#2985=ORIENTED_EDGE('',*,*,#1958,.T.);
#2986=ORIENTED_EDGE('',*,*,#2009,.F.);
#2987=ORIENTED_EDGE('',*,*,#2067,.F.);
#2988=ORIENTED_EDGE('',*,*,#2160,.F.);
#2989=ORIENTED_EDGE('',*,*,#2115,.F.);
#2990=ORIENTED_EDGE('',*,*,#2053,.F.);
#2991=ORIENTED_EDGE('',*,*,#1995,.F.);
#2992=ORIENTED_EDGE('',*,*,#1940,.T.);
#2993=ORIENTED_EDGE('',*,*,#2121,.F.);
#2994=ORIENTED_EDGE('',*,*,#2059,.F.);
#2995=ORIENTED_EDGE('',*,*,#2001,.F.);
#2996=ORIENTED_EDGE('',*,*,#1948,.T.);
#2997=ORIENTED_EDGE('',*,*,#2125,.F.);
#2998=ORIENTED_EDGE('',*,*,#2065,.F.);
#2999=ORIENTED_EDGE('',*,*,#2007,.F.);
#3000=ORIENTED_EDGE('',*,*,#1956,.T.);
#3001=ORIENTED_EDGE('',*,*,#2129,.F.);
#3002=ORIENTED_EDGE('',*,*,#2071,.F.);
#3003=ORIENTED_EDGE('',*,*,#2013,.F.);
#3004=ORIENTED_EDGE('',*,*,#1932,.T.);
#3005=ORIENTED_EDGE('',*,*,#2152,.F.);
#3006=ORIENTED_EDGE('',*,*,#2108,.F.);
#3007=ORIENTED_EDGE('',*,*,#2185,.F.);
#3008=ORIENTED_EDGE('',*,*,#2167,.T.);
#3009=ORIENTED_EDGE('',*,*,#2213,.F.);
#3010=ORIENTED_EDGE('',*,*,#2202,.F.);
#3011=ORIENTED_EDGE('',*,*,#2192,.F.);
#3012=ORIENTED_EDGE('',*,*,#2219,.T.);
#3013=ORIENTED_EDGE('',*,*,#1923,.F.);
#3014=ORIENTED_EDGE('',*,*,#2218,.F.);
#3015=ORIENTED_EDGE('',*,*,#2188,.F.);
#3016=ORIENTED_EDGE('',*,*,#2200,.F.);
#3017=ORIENTED_EDGE('',*,*,#2206,.F.);
#3018=ORIENTED_EDGE('',*,*,#2171,.T.);
#3019=ORIENTED_EDGE('',*,*,#2181,.F.);
#3020=ORIENTED_EDGE('',*,*,#2103,.F.);
#3021=ORIENTED_EDGE('',*,*,#2150,.F.);
#3022=ORIENTED_EDGE('',*,*,#1928,.T.);
#3023=ORIENTED_EDGE('',*,*,#2011,.F.);
#3024=ORIENTED_EDGE('',*,*,#2069,.F.);
#3025=ORIENTED_EDGE('',*,*,#2127,.F.);
#3026=ORIENTED_EDGE('',*,*,#1952,.T.);
#3027=ORIENTED_EDGE('',*,*,#2005,.F.);
#3028=ORIENTED_EDGE('',*,*,#2063,.F.);
#3029=ORIENTED_EDGE('',*,*,#2123,.F.);
#3030=ORIENTED_EDGE('',*,*,#1944,.T.);
#3031=ORIENTED_EDGE('',*,*,#1999,.F.);
#3032=ORIENTED_EDGE('',*,*,#2057,.F.);
#3033=ORIENTED_EDGE('',*,*,#2119,.F.);
#3034=ORIENTED_EDGE('',*,*,#1936,.T.);
#3035=ORIENTED_EDGE('',*,*,#1993,.F.);
#3036=ORIENTED_EDGE('',*,*,#2051,.F.);
#3037=ORIENTED_EDGE('',*,*,#2112,.F.);
#3038=ORIENTED_EDGE('',*,*,#2157,.F.);
#3039=ORIENTED_EDGE('',*,*,#1925,.F.);
#3040=ORIENTED_EDGE('',*,*,#2217,.T.);
#3041=ORIENTED_EDGE('',*,*,#2211,.F.);
#3042=ORIENTED_EDGE('',*,*,#2169,.T.);
#3043=ORIENTED_EDGE('',*,*,#2184,.F.);
#3044=ORIENTED_EDGE('',*,*,#2197,.F.);
#3045=ORIENTED_EDGE('',*,*,#2209,.F.);
#3046=ORIENTED_EDGE('',*,*,#2178,.T.);
#3047=ORIENTED_EDGE('',*,*,#2046,.F.);
#3048=ORIENTED_EDGE('',*,*,#2100,.F.);
#3049=ORIENTED_EDGE('',*,*,#2148,.F.);
#3050=ORIENTED_EDGE('',*,*,#1988,.T.);
#3051=ORIENTED_EDGE('',*,*,#2039,.F.);
#3052=ORIENTED_EDGE('',*,*,#2093,.F.);
#3053=ORIENTED_EDGE('',*,*,#2144,.F.);
#3054=ORIENTED_EDGE('',*,*,#1980,.T.);
#3055=ORIENTED_EDGE('',*,*,#2033,.F.);
#3056=ORIENTED_EDGE('',*,*,#2087,.F.);
#3057=ORIENTED_EDGE('',*,*,#2140,.F.);
#3058=ORIENTED_EDGE('',*,*,#1972,.T.);
#3059=ORIENTED_EDGE('',*,*,#2027,.F.);
#3060=ORIENTED_EDGE('',*,*,#2081,.F.);
#3061=ORIENTED_EDGE('',*,*,#2136,.F.);
#3062=ORIENTED_EDGE('',*,*,#1964,.T.);
#3063=ORIENTED_EDGE('',*,*,#2165,.F.);
#3064=ORIENTED_EDGE('',*,*,#1914,.F.);
#3065=ORIENTED_EDGE('',*,*,#2163,.F.);
#3066=ORIENTED_EDGE('',*,*,#2017,.F.);
#3067=ORIENTED_EDGE('',*,*,#1960,.T.);
#3068=ORIENTED_EDGE('',*,*,#2134,.F.);
#3069=ORIENTED_EDGE('',*,*,#2077,.F.);
#3070=ORIENTED_EDGE('',*,*,#2023,.F.);
#3071=ORIENTED_EDGE('',*,*,#1968,.T.);
#3072=ORIENTED_EDGE('',*,*,#2138,.F.);
#3073=ORIENTED_EDGE('',*,*,#2083,.F.);
#3074=ORIENTED_EDGE('',*,*,#2029,.F.);
#3075=ORIENTED_EDGE('',*,*,#1976,.T.);
#3076=ORIENTED_EDGE('',*,*,#2142,.F.);
#3077=ORIENTED_EDGE('',*,*,#2089,.F.);
#3078=ORIENTED_EDGE('',*,*,#2035,.F.);
#3079=ORIENTED_EDGE('',*,*,#1984,.T.);
#3080=ORIENTED_EDGE('',*,*,#2146,.F.);
#3081=ORIENTED_EDGE('',*,*,#2095,.F.);
#3082=ORIENTED_EDGE('',*,*,#2042,.F.);
#3083=ORIENTED_EDGE('',*,*,#2175,.T.);
#3084=ORIENTED_EDGE('',*,*,#2207,.F.);
#3085=ORIENTED_EDGE('',*,*,#2201,.F.);
#3086=ORIENTED_EDGE('',*,*,#2190,.F.);
#3087=ORIENTED_EDGE('',*,*,#1908,.T.);
#3088=ORIENTED_EDGE('',*,*,#2214,.F.);
#3089=ORIENTED_EDGE('',*,*,#1912,.F.);
#3090=ORIENTED_EDGE('',*,*,#2154,.T.);
#3091=ORIENTED_EDGE('',*,*,#2131,.F.);
#3092=ORIENTED_EDGE('',*,*,#2074,.F.);
#3093=ORIENTED_EDGE('',*,*,#2020,.F.);
#3094=ORIENTED_EDGE('',*,*,#1891,.T.);
#3095=ORIENTED_EDGE('',*,*,#1919,.F.);
#3096=ORIENTED_EDGE('',*,*,#2230,.T.);
#3097=ORIENTED_EDGE('',*,*,#2231,.T.);
#3098=ORIENTED_EDGE('',*,*,#2232,.F.);
#3099=ORIENTED_EDGE('',*,*,#2233,.F.);
#3100=ORIENTED_EDGE('',*,*,#2234,.F.);
#3101=ORIENTED_EDGE('',*,*,#2235,.T.);
#3102=ORIENTED_EDGE('',*,*,#2236,.T.);
#3103=ORIENTED_EDGE('',*,*,#2230,.F.);
#3104=ORIENTED_EDGE('',*,*,#2237,.F.);
#3105=ORIENTED_EDGE('',*,*,#2238,.T.);
#3106=ORIENTED_EDGE('',*,*,#2239,.T.);
#3107=ORIENTED_EDGE('',*,*,#2235,.F.);
#3108=ORIENTED_EDGE('',*,*,#2240,.F.);
#3109=ORIENTED_EDGE('',*,*,#2241,.F.);
#3110=ORIENTED_EDGE('',*,*,#2242,.F.);
#3111=ORIENTED_EDGE('',*,*,#2243,.F.);
#3112=ORIENTED_EDGE('',*,*,#2244,.T.);
#3113=ORIENTED_EDGE('',*,*,#2245,.T.);
#3114=ORIENTED_EDGE('',*,*,#2246,.F.);
#3115=ORIENTED_EDGE('',*,*,#2247,.T.);
#3116=ORIENTED_EDGE('',*,*,#2248,.T.);
#3117=ORIENTED_EDGE('',*,*,#2249,.F.);
#3118=ORIENTED_EDGE('',*,*,#2250,.F.);
#3119=ORIENTED_EDGE('',*,*,#2251,.F.);
#3120=ORIENTED_EDGE('',*,*,#2245,.F.);
#3121=ORIENTED_EDGE('',*,*,#2252,.T.);
#3122=ORIENTED_EDGE('',*,*,#2253,.T.);
#3123=ORIENTED_EDGE('',*,*,#2254,.F.);
#3124=ORIENTED_EDGE('',*,*,#2248,.F.);
#3125=ORIENTED_EDGE('',*,*,#2255,.T.);
#3126=ORIENTED_EDGE('',*,*,#2256,.F.);
#3127=ORIENTED_EDGE('',*,*,#2257,.T.);
#3128=ORIENTED_EDGE('',*,*,#2258,.F.);
#3129=ORIENTED_EDGE('',*,*,#2259,.T.);
#3130=ORIENTED_EDGE('',*,*,#2260,.F.);
#3131=ORIENTED_EDGE('',*,*,#2261,.F.);
#3132=ORIENTED_EDGE('',*,*,#2262,.T.);
#3133=ORIENTED_EDGE('',*,*,#2263,.T.);
#3134=ORIENTED_EDGE('',*,*,#2262,.F.);
#3135=ORIENTED_EDGE('',*,*,#2264,.F.);
#3136=ORIENTED_EDGE('',*,*,#2265,.T.);
#3137=ORIENTED_EDGE('',*,*,#2266,.T.);
#3138=ORIENTED_EDGE('',*,*,#2265,.F.);
#3139=ORIENTED_EDGE('',*,*,#2267,.T.);
#3140=ORIENTED_EDGE('',*,*,#2268,.T.);
#3141=ORIENTED_EDGE('',*,*,#2269,.F.);
#3142=ORIENTED_EDGE('',*,*,#2268,.F.);
#3143=ORIENTED_EDGE('',*,*,#2270,.T.);
#3144=ORIENTED_EDGE('',*,*,#2271,.T.);
#3145=ORIENTED_EDGE('',*,*,#2272,.F.);
#3146=ORIENTED_EDGE('',*,*,#2271,.F.);
#3147=ORIENTED_EDGE('',*,*,#2256,.T.);
#3148=ORIENTED_EDGE('',*,*,#2273,.F.);
#3149=ORIENTED_EDGE('',*,*,#2253,.F.);
#3150=ORIENTED_EDGE('',*,*,#2274,.T.);
#3151=ORIENTED_EDGE('',*,*,#2275,.F.);
#3152=ORIENTED_EDGE('',*,*,#2258,.T.);
#3153=ORIENTED_EDGE('',*,*,#2276,.T.);
#3154=ORIENTED_EDGE('',*,*,#2233,.T.);
#3155=ORIENTED_EDGE('',*,*,#2241,.T.);
#3156=ORIENTED_EDGE('',*,*,#2277,.T.);
#3157=ORIENTED_EDGE('',*,*,#2238,.F.);
#3158=ORIENTED_EDGE('',*,*,#2278,.F.);
#3159=ORIENTED_EDGE('',*,*,#2279,.F.);
#3160=ORIENTED_EDGE('',*,*,#2231,.F.);
#3161=ORIENTED_EDGE('',*,*,#2236,.F.);
#3162=ORIENTED_EDGE('',*,*,#2239,.F.);
#3163=ORIENTED_EDGE('',*,*,#2277,.F.);
#3164=ORIENTED_EDGE('',*,*,#2244,.F.);
#3165=ORIENTED_EDGE('',*,*,#2280,.F.);
#3166=ORIENTED_EDGE('',*,*,#2249,.T.);
#3167=ORIENTED_EDGE('',*,*,#2254,.T.);
#3168=ORIENTED_EDGE('',*,*,#2273,.T.);
#3169=ORIENTED_EDGE('',*,*,#2260,.T.);
#3170=ORIENTED_EDGE('',*,*,#2269,.T.);
#3171=ORIENTED_EDGE('',*,*,#2266,.F.);
#3172=ORIENTED_EDGE('',*,*,#2267,.F.);
#3173=ORIENTED_EDGE('',*,*,#2246,.T.);
#3174=ORIENTED_EDGE('',*,*,#2251,.T.);
#3175=ORIENTED_EDGE('',*,*,#2281,.T.);
#3176=ORIENTED_EDGE('',*,*,#2250,.T.);
#3177=ORIENTED_EDGE('',*,*,#2280,.T.);
#3178=ORIENTED_EDGE('',*,*,#2243,.T.);
#3179=ORIENTED_EDGE('',*,*,#2281,.F.);
#3180=ORIENTED_EDGE('',*,*,#2242,.T.);
#3181=ORIENTED_EDGE('',*,*,#2278,.T.);
#3182=ORIENTED_EDGE('',*,*,#2240,.T.);
#3183=ORIENTED_EDGE('',*,*,#2237,.T.);
#3184=ORIENTED_EDGE('',*,*,#2234,.T.);
#3185=ORIENTED_EDGE('',*,*,#2276,.F.);
#3186=ORIENTED_EDGE('',*,*,#2257,.F.);
#3187=ORIENTED_EDGE('',*,*,#2274,.F.);
#3188=ORIENTED_EDGE('',*,*,#2255,.F.);
#3189=ORIENTED_EDGE('',*,*,#2252,.F.);
#3190=ORIENTED_EDGE('',*,*,#2247,.F.);
#3191=ORIENTED_EDGE('',*,*,#2264,.T.);
#3192=ORIENTED_EDGE('',*,*,#2270,.F.);
#3193=ORIENTED_EDGE('',*,*,#2261,.T.);
#3194=ORIENTED_EDGE('',*,*,#2275,.T.);
#3195=ORIENTED_EDGE('',*,*,#2232,.T.);
#3196=ORIENTED_EDGE('',*,*,#2279,.T.);
#3197=ORIENTED_EDGE('',*,*,#2259,.F.);
#3198=ORIENTED_EDGE('',*,*,#2263,.F.);
#3199=ORIENTED_EDGE('',*,*,#2272,.T.);
#3200=ORIENTED_EDGE('',*,*,#2282,.T.);
#3201=ORIENTED_EDGE('',*,*,#2283,.T.);
#3202=ORIENTED_EDGE('',*,*,#2284,.F.);
#3203=ORIENTED_EDGE('',*,*,#2283,.F.);
#3204=ORIENTED_EDGE('',*,*,#2284,.T.);
#3205=ORIENTED_EDGE('',*,*,#2282,.F.);
#3206=ORIENTED_EDGE('',*,*,#2285,.T.);
#3207=ORIENTED_EDGE('',*,*,#2286,.T.);
#3208=ORIENTED_EDGE('',*,*,#2287,.F.);
#3209=ORIENTED_EDGE('',*,*,#2286,.F.);
#3210=ORIENTED_EDGE('',*,*,#2288,.T.);
#3211=ORIENTED_EDGE('',*,*,#2289,.T.);
#3212=ORIENTED_EDGE('',*,*,#2290,.F.);
#3213=ORIENTED_EDGE('',*,*,#2289,.F.);
#3214=ORIENTED_EDGE('',*,*,#2290,.T.);
#3215=ORIENTED_EDGE('',*,*,#2285,.F.);
#3216=ORIENTED_EDGE('',*,*,#2288,.F.);
#3217=ORIENTED_EDGE('',*,*,#2287,.T.);
#3218=ORIENTED_EDGE('',*,*,#2291,.T.);
#3219=ORIENTED_EDGE('',*,*,#2292,.T.);
#3220=ORIENTED_EDGE('',*,*,#2293,.F.);
#3221=ORIENTED_EDGE('',*,*,#2292,.F.);
#3222=ORIENTED_EDGE('',*,*,#2294,.T.);
#3223=ORIENTED_EDGE('',*,*,#2295,.T.);
#3224=ORIENTED_EDGE('',*,*,#2296,.F.);
#3225=ORIENTED_EDGE('',*,*,#2295,.F.);
#3226=ORIENTED_EDGE('',*,*,#2296,.T.);
#3227=ORIENTED_EDGE('',*,*,#2291,.F.);
#3228=ORIENTED_EDGE('',*,*,#2294,.F.);
#3229=ORIENTED_EDGE('',*,*,#2293,.T.);
#3230=ORIENTED_EDGE('',*,*,#2297,.F.);
#3231=ORIENTED_EDGE('',*,*,#2298,.T.);
#3232=ORIENTED_EDGE('',*,*,#2299,.T.);
#3233=ORIENTED_EDGE('',*,*,#2298,.F.);
#3234=ORIENTED_EDGE('',*,*,#2300,.F.);
#3235=ORIENTED_EDGE('',*,*,#2301,.T.);
#3236=ORIENTED_EDGE('',*,*,#2302,.T.);
#3237=ORIENTED_EDGE('',*,*,#2301,.F.);
#3238=ORIENTED_EDGE('',*,*,#2303,.T.);
#3239=ORIENTED_EDGE('',*,*,#2304,.T.);
#3240=ORIENTED_EDGE('',*,*,#2305,.F.);
#3241=ORIENTED_EDGE('',*,*,#2304,.F.);
#3242=ORIENTED_EDGE('',*,*,#2306,.T.);
#3243=ORIENTED_EDGE('',*,*,#2307,.T.);
#3244=ORIENTED_EDGE('',*,*,#2308,.F.);
#3245=ORIENTED_EDGE('',*,*,#2307,.F.);
#3246=ORIENTED_EDGE('',*,*,#2309,.T.);
#3247=ORIENTED_EDGE('',*,*,#2310,.T.);
#3248=ORIENTED_EDGE('',*,*,#2311,.F.);
#3249=ORIENTED_EDGE('',*,*,#2310,.F.);
#3250=ORIENTED_EDGE('',*,*,#2312,.T.);
#3251=ORIENTED_EDGE('',*,*,#2313,.T.);
#3252=ORIENTED_EDGE('',*,*,#2314,.F.);
#3253=ORIENTED_EDGE('',*,*,#2313,.F.);
#3254=ORIENTED_EDGE('',*,*,#2315,.T.);
#3255=ORIENTED_EDGE('',*,*,#2316,.T.);
#3256=ORIENTED_EDGE('',*,*,#2317,.F.);
#3257=ORIENTED_EDGE('',*,*,#2316,.F.);
#3258=ORIENTED_EDGE('',*,*,#2317,.T.);
#3259=ORIENTED_EDGE('',*,*,#2309,.F.);
#3260=ORIENTED_EDGE('',*,*,#2303,.F.);
#3261=ORIENTED_EDGE('',*,*,#2302,.F.);
#3262=ORIENTED_EDGE('',*,*,#2306,.F.);
#3263=ORIENTED_EDGE('',*,*,#2312,.F.);
#3264=ORIENTED_EDGE('',*,*,#2315,.F.);
#3265=ORIENTED_EDGE('',*,*,#2314,.T.);
#3266=ORIENTED_EDGE('',*,*,#2311,.T.);
#3267=ORIENTED_EDGE('',*,*,#2308,.T.);
#3268=ORIENTED_EDGE('',*,*,#2305,.T.);
#3269=ORIENTED_EDGE('',*,*,#2297,.T.);
#3270=ORIENTED_EDGE('',*,*,#2300,.T.);
#3271=ORIENTED_EDGE('',*,*,#2299,.F.);
#3272=ORIENTED_EDGE('',*,*,#2318,.T.);
#3273=ORIENTED_EDGE('',*,*,#2319,.T.);
#3274=ORIENTED_EDGE('',*,*,#2320,.T.);
#3275=ORIENTED_EDGE('',*,*,#2321,.T.);
#3276=ORIENTED_EDGE('',*,*,#2322,.T.);
#3277=ORIENTED_EDGE('',*,*,#2323,.T.);
#3278=ORIENTED_EDGE('',*,*,#2324,.T.);
#3279=ORIENTED_EDGE('',*,*,#2325,.T.);
#3280=ORIENTED_EDGE('',*,*,#2326,.T.);
#3281=ORIENTED_EDGE('',*,*,#2327,.T.);
#3282=ORIENTED_EDGE('',*,*,#2328,.T.);
#3283=ORIENTED_EDGE('',*,*,#2329,.T.);
#3284=ORIENTED_EDGE('',*,*,#2330,.T.);
#3285=ORIENTED_EDGE('',*,*,#2331,.T.);
#3286=ORIENTED_EDGE('',*,*,#2332,.T.);
#3287=ORIENTED_EDGE('',*,*,#2333,.T.);
#3288=ORIENTED_EDGE('',*,*,#2334,.T.);
#3289=ORIENTED_EDGE('',*,*,#2335,.T.);
#3290=ORIENTED_EDGE('',*,*,#2336,.T.);
#3291=ORIENTED_EDGE('',*,*,#2337,.T.);
#3292=ORIENTED_EDGE('',*,*,#2338,.T.);
#3293=ORIENTED_EDGE('',*,*,#2339,.T.);
#3294=ORIENTED_EDGE('',*,*,#2340,.T.);
#3295=ORIENTED_EDGE('',*,*,#2341,.T.);
#3296=ORIENTED_EDGE('',*,*,#2342,.F.);
#3297=ORIENTED_EDGE('',*,*,#2324,.F.);
#3298=ORIENTED_EDGE('',*,*,#2343,.F.);
#3299=ORIENTED_EDGE('',*,*,#2326,.F.);
#3300=ORIENTED_EDGE('',*,*,#2344,.F.);
#3301=ORIENTED_EDGE('',*,*,#2342,.T.);
#3302=ORIENTED_EDGE('',*,*,#2345,.F.);
#3303=ORIENTED_EDGE('',*,*,#2346,.F.);
#3304=ORIENTED_EDGE('',*,*,#2343,.T.);
#3305=ORIENTED_EDGE('',*,*,#2347,.F.);
#3306=ORIENTED_EDGE('',*,*,#2345,.T.);
#3307=ORIENTED_EDGE('',*,*,#2329,.F.);
#3308=ORIENTED_EDGE('',*,*,#2348,.F.);
#3309=ORIENTED_EDGE('',*,*,#2334,.F.);
#3310=ORIENTED_EDGE('',*,*,#2344,.T.);
#3311=ORIENTED_EDGE('',*,*,#2337,.F.);
#3312=ORIENTED_EDGE('',*,*,#2349,.F.);
#3313=ORIENTED_EDGE('',*,*,#2325,.F.);
#3314=ORIENTED_EDGE('',*,*,#2350,.F.);
#3315=ORIENTED_EDGE('',*,*,#2322,.F.);
#3316=ORIENTED_EDGE('',*,*,#2351,.F.);
#3317=ORIENTED_EDGE('',*,*,#2320,.F.);
#3318=ORIENTED_EDGE('',*,*,#2347,.T.);
#3319=ORIENTED_EDGE('',*,*,#2323,.F.);
#3320=ORIENTED_EDGE('',*,*,#2352,.F.);
#3321=ORIENTED_EDGE('',*,*,#2339,.F.);
#3322=ORIENTED_EDGE('',*,*,#2346,.T.);
#3323=ORIENTED_EDGE('',*,*,#2338,.F.);
#3324=ORIENTED_EDGE('',*,*,#2353,.F.);
#3325=ORIENTED_EDGE('',*,*,#2327,.F.);
#3326=ORIENTED_EDGE('',*,*,#2354,.F.);
#3327=ORIENTED_EDGE('',*,*,#2328,.F.);
#3328=ORIENTED_EDGE('',*,*,#2355,.F.);
#3329=ORIENTED_EDGE('',*,*,#2330,.F.);
#3330=ORIENTED_EDGE('',*,*,#2348,.T.);
#3331=ORIENTED_EDGE('',*,*,#2354,.T.);
#3332=ORIENTED_EDGE('',*,*,#2356,.F.);
#3333=ORIENTED_EDGE('',*,*,#2351,.T.);
#3334=ORIENTED_EDGE('',*,*,#2349,.T.);
#3335=ORIENTED_EDGE('',*,*,#2357,.F.);
#3336=ORIENTED_EDGE('',*,*,#2352,.T.);
#3337=ORIENTED_EDGE('',*,*,#2350,.T.);
#3338=ORIENTED_EDGE('',*,*,#2358,.F.);
#3339=ORIENTED_EDGE('',*,*,#2355,.T.);
#3340=ORIENTED_EDGE('',*,*,#2353,.T.);
#3341=ORIENTED_EDGE('',*,*,#2359,.F.);
#3342=ORIENTED_EDGE('',*,*,#2356,.T.);
#3343=ORIENTED_EDGE('',*,*,#2333,.F.);
#3344=ORIENTED_EDGE('',*,*,#2360,.F.);
#3345=ORIENTED_EDGE('',*,*,#2335,.F.);
#3346=ORIENTED_EDGE('',*,*,#2357,.T.);
#3347=ORIENTED_EDGE('',*,*,#2336,.F.);
#3348=ORIENTED_EDGE('',*,*,#2361,.F.);
#3349=ORIENTED_EDGE('',*,*,#2321,.F.);
#3350=ORIENTED_EDGE('',*,*,#2358,.T.);
#3351=ORIENTED_EDGE('',*,*,#2319,.F.);
#3352=ORIENTED_EDGE('',*,*,#2362,.F.);
#3353=ORIENTED_EDGE('',*,*,#2340,.F.);
#3354=ORIENTED_EDGE('',*,*,#2359,.T.);
#3355=ORIENTED_EDGE('',*,*,#2341,.F.);
#3356=ORIENTED_EDGE('',*,*,#2363,.F.);
#3357=ORIENTED_EDGE('',*,*,#2331,.F.);
#3358=ORIENTED_EDGE('',*,*,#2361,.T.);
#3359=ORIENTED_EDGE('',*,*,#2360,.T.);
#3360=ORIENTED_EDGE('',*,*,#2364,.F.);
#3361=ORIENTED_EDGE('',*,*,#2363,.T.);
#3362=ORIENTED_EDGE('',*,*,#2362,.T.);
#3363=ORIENTED_EDGE('',*,*,#2365,.F.);
#3364=ORIENTED_EDGE('',*,*,#2364,.T.);
#3365=ORIENTED_EDGE('',*,*,#2332,.F.);
#3366=ORIENTED_EDGE('',*,*,#2365,.T.);
#3367=ORIENTED_EDGE('',*,*,#2318,.F.);
#3368=ORIENTED_EDGE('',*,*,#2366,.T.);
#3369=ORIENTED_EDGE('',*,*,#2367,.T.);
#3370=ORIENTED_EDGE('',*,*,#2368,.F.);
#3371=ORIENTED_EDGE('',*,*,#2367,.F.);
#3372=ORIENTED_EDGE('',*,*,#2368,.T.);
#3373=ORIENTED_EDGE('',*,*,#2366,.F.);
#3374=ORIENTED_EDGE('',*,*,#2369,.F.);
#3375=ORIENTED_EDGE('',*,*,#2370,.F.);
#3376=ORIENTED_EDGE('',*,*,#2371,.F.);
#3377=ORIENTED_EDGE('',*,*,#2372,.F.);
#3378=ORIENTED_EDGE('',*,*,#2373,.F.);
#3379=ORIENTED_EDGE('',*,*,#2374,.T.);
#3380=ORIENTED_EDGE('',*,*,#2375,.F.);
#3381=ORIENTED_EDGE('',*,*,#2376,.F.);
#3382=ORIENTED_EDGE('',*,*,#2377,.F.);
#3383=ORIENTED_EDGE('',*,*,#2369,.T.);
#3384=ORIENTED_EDGE('',*,*,#2378,.F.);
#3385=ORIENTED_EDGE('',*,*,#2379,.F.);
#3386=ORIENTED_EDGE('',*,*,#2380,.F.);
#3387=ORIENTED_EDGE('',*,*,#2374,.F.);
#3388=ORIENTED_EDGE('',*,*,#2381,.T.);
#3389=ORIENTED_EDGE('',*,*,#2382,.T.);
#3390=ORIENTED_EDGE('',*,*,#2383,.T.);
#3391=ORIENTED_EDGE('',*,*,#2384,.T.);
#3392=ORIENTED_EDGE('',*,*,#2385,.F.);
#3393=ORIENTED_EDGE('',*,*,#2386,.T.);
#3394=ORIENTED_EDGE('',*,*,#2387,.T.);
#3395=ORIENTED_EDGE('',*,*,#2388,.T.);
#3396=ORIENTED_EDGE('',*,*,#2389,.T.);
#3397=ORIENTED_EDGE('',*,*,#2390,.T.);
#3398=ORIENTED_EDGE('',*,*,#2391,.F.);
#3399=ORIENTED_EDGE('',*,*,#2384,.F.);
#3400=ORIENTED_EDGE('',*,*,#2392,.T.);
#3401=ORIENTED_EDGE('',*,*,#2393,.T.);
#3402=ORIENTED_EDGE('',*,*,#2394,.T.);
#3403=ORIENTED_EDGE('',*,*,#2392,.F.);
#3404=ORIENTED_EDGE('',*,*,#2383,.F.);
#3405=ORIENTED_EDGE('',*,*,#2395,.T.);
#3406=ORIENTED_EDGE('',*,*,#2381,.F.);
#3407=ORIENTED_EDGE('',*,*,#2396,.F.);
#3408=ORIENTED_EDGE('',*,*,#2371,.T.);
#3409=ORIENTED_EDGE('',*,*,#2397,.F.);
#3410=ORIENTED_EDGE('',*,*,#2385,.T.);
#3411=ORIENTED_EDGE('',*,*,#2391,.T.);
#3412=ORIENTED_EDGE('',*,*,#2398,.T.);
#3413=ORIENTED_EDGE('',*,*,#2379,.T.);
#3414=ORIENTED_EDGE('',*,*,#2399,.F.);
#3415=ORIENTED_EDGE('',*,*,#2389,.F.);
#3416=ORIENTED_EDGE('',*,*,#2400,.T.);
#3417=ORIENTED_EDGE('',*,*,#2375,.T.);
#3418=ORIENTED_EDGE('',*,*,#2380,.T.);
#3419=ORIENTED_EDGE('',*,*,#2398,.F.);
#3420=ORIENTED_EDGE('',*,*,#2388,.F.);
#3421=ORIENTED_EDGE('',*,*,#2401,.T.);
#3422=ORIENTED_EDGE('',*,*,#2376,.T.);
#3423=ORIENTED_EDGE('',*,*,#2400,.F.);
#3424=ORIENTED_EDGE('',*,*,#2387,.F.);
#3425=ORIENTED_EDGE('',*,*,#2397,.T.);
#3426=ORIENTED_EDGE('',*,*,#2370,.T.);
#3427=ORIENTED_EDGE('',*,*,#2377,.T.);
#3428=ORIENTED_EDGE('',*,*,#2401,.F.);
#3429=ORIENTED_EDGE('',*,*,#2386,.F.);
#3430=ORIENTED_EDGE('',*,*,#2378,.T.);
#3431=ORIENTED_EDGE('',*,*,#2372,.T.);
#3432=ORIENTED_EDGE('',*,*,#2396,.T.);
#3433=ORIENTED_EDGE('',*,*,#2390,.F.);
#3434=ORIENTED_EDGE('',*,*,#2399,.T.);
#3435=ORIENTED_EDGE('',*,*,#2395,.F.);
#3436=ORIENTED_EDGE('',*,*,#2393,.F.);
#3437=ORIENTED_EDGE('',*,*,#2394,.F.);
#3438=ORIENTED_EDGE('',*,*,#2382,.F.);
#3439=ORIENTED_EDGE('',*,*,#2373,.T.);
#3440=TOROIDAL_SURFACE('',#3798,150.,3.96875);
#3441=TOROIDAL_SURFACE('',#4101,150.,3.96875);
#3442=ADVANCED_FACE('',(#980),#3440,.T.);
#3443=ADVANCED_FACE('',(#981),#834,.T.);
#3444=ADVANCED_FACE('',(#982),#393,.T.);
#3445=ADVANCED_FACE('',(#983),#394,.F.);
#3446=ADVANCED_FACE('',(#984),#835,.T.);
#3447=ADVANCED_FACE('',(#985),#395,.T.);
#3448=ADVANCED_FACE('',(#986),#396,.F.);
#3449=ADVANCED_FACE('',(#987),#836,.F.);
#3450=ADVANCED_FACE('',(#988),#837,.T.);
#3451=ADVANCED_FACE('',(#989),#838,.T.);
#3452=ADVANCED_FACE('',(#990),#839,.T.);
#3453=ADVANCED_FACE('',(#991),#840,.F.);
#3454=ADVANCED_FACE('',(#992),#841,.T.);
#3455=ADVANCED_FACE('',(#993),#842,.T.);
#3456=ADVANCED_FACE('',(#994),#843,.T.);
#3457=ADVANCED_FACE('',(#995),#844,.T.);
#3458=ADVANCED_FACE('',(#996),#845,.T.);
#3459=ADVANCED_FACE('',(#997),#846,.T.);
#3460=ADVANCED_FACE('',(#998),#847,.T.);
#3461=ADVANCED_FACE('',(#999),#848,.T.);
#3462=ADVANCED_FACE('',(#1000),#849,.T.);
#3463=ADVANCED_FACE('',(#1001),#850,.T.);
#3464=ADVANCED_FACE('',(#1002),#851,.T.);
#3465=ADVANCED_FACE('',(#1003),#852,.T.);
#3466=ADVANCED_FACE('',(#1004),#853,.T.);
#3467=ADVANCED_FACE('',(#1005),#854,.T.);
#3468=ADVANCED_FACE('',(#1006),#855,.T.);
#3469=ADVANCED_FACE('',(#1007),#856,.T.);
#3470=ADVANCED_FACE('',(#1008),#152,.T.);
#3471=ADVANCED_FACE('',(#1009),#153,.T.);
#3472=ADVANCED_FACE('',(#1010),#154,.T.);
#3473=ADVANCED_FACE('',(#1011),#155,.T.);
#3474=ADVANCED_FACE('',(#1012),#156,.T.);
#3475=ADVANCED_FACE('',(#1013),#157,.T.);
#3476=ADVANCED_FACE('',(#1014),#158,.T.);
#3477=ADVANCED_FACE('',(#1015),#159,.T.);
#3478=ADVANCED_FACE('',(#1016),#160,.T.);
#3479=ADVANCED_FACE('',(#1017),#161,.T.);
#3480=ADVANCED_FACE('',(#1018),#162,.T.);
#3481=ADVANCED_FACE('',(#1019),#163,.T.);
#3482=ADVANCED_FACE('',(#1020),#164,.T.);
#3483=ADVANCED_FACE('',(#1021),#165,.T.);
#3484=ADVANCED_FACE('',(#1022),#166,.T.);
#3485=ADVANCED_FACE('',(#1023),#167,.T.);
#3486=ADVANCED_FACE('',(#1024),#168,.T.);
#3487=ADVANCED_FACE('',(#1025),#857,.T.);
#3488=ADVANCED_FACE('',(#1026),#858,.T.);
#3489=ADVANCED_FACE('',(#1027),#859,.T.);
#3490=ADVANCED_FACE('',(#1028),#860,.T.);
#3491=ADVANCED_FACE('',(#1029),#861,.T.);
#3492=ADVANCED_FACE('',(#1030),#862,.T.);
#3493=ADVANCED_FACE('',(#1031),#863,.T.);
#3494=ADVANCED_FACE('',(#1032),#864,.T.);
#3495=ADVANCED_FACE('',(#1033),#865,.T.);
#3496=ADVANCED_FACE('',(#1034),#866,.T.);
#3497=ADVANCED_FACE('',(#1035),#867,.T.);
#3498=ADVANCED_FACE('',(#1036),#868,.T.);
#3499=ADVANCED_FACE('',(#1037),#869,.T.);
#3500=ADVANCED_FACE('',(#1038),#870,.T.);
#3501=ADVANCED_FACE('',(#1039),#871,.T.);
#3502=ADVANCED_FACE('',(#1040),#872,.T.);
#3503=ADVANCED_FACE('',(#1041),#873,.T.);
#3504=ADVANCED_FACE('',(#1042),#874,.T.);
#3505=ADVANCED_FACE('',(#1043),#875,.T.);
#3506=ADVANCED_FACE('',(#1044),#169,.T.);
#3507=ADVANCED_FACE('',(#1045),#170,.T.);
#3508=ADVANCED_FACE('',(#1046),#171,.T.);
#3509=ADVANCED_FACE('',(#1047),#172,.T.);
#3510=ADVANCED_FACE('',(#1048),#173,.T.);
#3511=ADVANCED_FACE('',(#1049),#174,.T.);
#3512=ADVANCED_FACE('',(#1050),#175,.T.);
#3513=ADVANCED_FACE('',(#1051),#176,.T.);
#3514=ADVANCED_FACE('',(#1052),#177,.T.);
#3515=ADVANCED_FACE('',(#1053),#178,.T.);
#3516=ADVANCED_FACE('',(#1054),#179,.T.);
#3517=ADVANCED_FACE('',(#1055),#180,.T.);
#3518=ADVANCED_FACE('',(#1056),#181,.T.);
#3519=ADVANCED_FACE('',(#1057),#182,.T.);
#3520=ADVANCED_FACE('',(#1058),#183,.T.);
#3521=ADVANCED_FACE('',(#1059),#184,.T.);
#3522=ADVANCED_FACE('',(#1060),#185,.T.);
#3523=ADVANCED_FACE('',(#1061),#186,.T.);
#3524=ADVANCED_FACE('',(#1062),#187,.T.);
#3525=ADVANCED_FACE('',(#1063),#876,.F.);
#3526=ADVANCED_FACE('',(#1064),#397,.T.);
#3527=ADVANCED_FACE('',(#1065),#398,.T.);
#3528=ADVANCED_FACE('',(#1066),#399,.T.);
#3529=ADVANCED_FACE('',(#1067),#400,.T.);
#3530=ADVANCED_FACE('',(#1068),#877,.T.);
#3531=ADVANCED_FACE('',(#1069),#878,.T.);
#3532=ADVANCED_FACE('',(#1070),#879,.T.);
#3533=ADVANCED_FACE('',(#1071),#880,.T.);
#3534=ADVANCED_FACE('',(#1072),#188,.T.);
#3535=ADVANCED_FACE('',(#1073),#189,.T.);
#3536=ADVANCED_FACE('',(#1074),#190,.T.);
#3537=ADVANCED_FACE('',(#1075),#191,.T.);
#3538=ADVANCED_FACE('',(#1076),#881,.T.);
#3539=ADVANCED_FACE('',(#1077),#882,.T.);
#3540=ADVANCED_FACE('',(#1078),#883,.T.);
#3541=ADVANCED_FACE('',(#1079),#192,.T.);
#3542=ADVANCED_FACE('',(#1080),#193,.T.);
#3543=ADVANCED_FACE('',(#1081),#194,.T.);
#3544=ADVANCED_FACE('',(#1082),#884,.F.);
#3545=ADVANCED_FACE('',(#1083),#885,.F.);
#3546=ADVANCED_FACE('',(#1084),#886,.T.);
#3547=ADVANCED_FACE('',(#1085),#887,.F.);
#3548=ADVANCED_FACE('',(#1086),#888,.F.);
#3549=ADVANCED_FACE('',(#1087),#889,.T.);
#3550=ADVANCED_FACE('',(#1088),#401,.T.);
#3551=ADVANCED_FACE('',(#1089),#402,.T.);
#3552=ADVANCED_FACE('',(#1090,#124),#403,.F.);
#3553=ADVANCED_FACE('',(#1091,#125),#404,.F.);
#3554=ADVANCED_FACE('',(#1092),#890,.F.);
#3555=ADVANCED_FACE('',(#1093),#405,.T.);
#3556=ADVANCED_FACE('',(#1094),#406,.T.);
#3557=ADVANCED_FACE('',(#1095),#407,.T.);
#3558=ADVANCED_FACE('',(#1096),#408,.T.);
#3559=ADVANCED_FACE('',(#1097),#409,.T.);
#3560=ADVANCED_FACE('',(#1098),#410,.T.);
#3561=ADVANCED_FACE('',(#1099),#411,.T.);
#3562=ADVANCED_FACE('',(#1100),#412,.T.);
#3563=ADVANCED_FACE('',(#1101),#413,.T.);
#3564=ADVANCED_FACE('',(#1102,#126),#414,.T.);
#3565=ADVANCED_FACE('',(#1103),#891,.F.);
#3566=ADVANCED_FACE('',(#1104),#892,.F.);
#3567=ADVANCED_FACE('',(#1105),#893,.F.);
#3568=ADVANCED_FACE('',(#1106),#894,.F.);
#3569=ADVANCED_FACE('',(#1107),#895,.F.);
#3570=ADVANCED_FACE('',(#1108),#896,.F.);
#3571=ADVANCED_FACE('',(#1109),#897,.F.);
#3572=ADVANCED_FACE('',(#1110),#898,.F.);
#3573=ADVANCED_FACE('',(#1111),#899,.F.);
#3574=ADVANCED_FACE('',(#1112),#900,.F.);
#3575=ADVANCED_FACE('',(#1113),#901,.T.);
#3576=ADVANCED_FACE('',(#1114),#902,.F.);
#3577=ADVANCED_FACE('',(#1115),#903,.F.);
#3578=ADVANCED_FACE('',(#1116),#415,.F.);
#3579=ADVANCED_FACE('',(#1117),#904,.F.);
#3580=ADVANCED_FACE('',(#1118),#195,.F.);
#3581=ADVANCED_FACE('',(#1119,#127),#416,.T.);
#3582=ADVANCED_FACE('',(#1120,#128),#417,.F.);
#3583=ADVANCED_FACE('',(#1121),#418,.T.);
#3584=ADVANCED_FACE('',(#1122),#196,.F.);
#3585=ADVANCED_FACE('',(#1123,#129),#419,.T.);
#3586=ADVANCED_FACE('',(#1124,#130),#420,.T.);
#3587=ADVANCED_FACE('',(#1125,#131),#421,.F.);
#3588=ADVANCED_FACE('',(#1126),#905,.T.);
#3589=ADVANCED_FACE('',(#1127),#422,.T.);
#3590=ADVANCED_FACE('',(#1128),#423,.F.);
#3591=ADVANCED_FACE('',(#1129),#906,.F.);
#3592=ADVANCED_FACE('',(#1130),#907,.T.);
#3593=ADVANCED_FACE('',(#1131,#132),#424,.T.);
#3594=ADVANCED_FACE('',(#1132,#133),#425,.F.);
#3595=ADVANCED_FACE('',(#1133),#908,.F.);
#3596=ADVANCED_FACE('',(#1134),#909,.T.);
#3597=ADVANCED_FACE('',(#1135,#134),#426,.T.);
#3598=ADVANCED_FACE('',(#1136,#135),#427,.F.);
#3599=ADVANCED_FACE('',(#1137),#910,.F.);
#3600=ADVANCED_FACE('',(#1138),#911,.F.);
#3601=ADVANCED_FACE('',(#1139),#912,.F.);
#3602=ADVANCED_FACE('',(#1140),#913,.F.);
#3603=ADVANCED_FACE('',(#1141),#914,.F.);
#3604=ADVANCED_FACE('',(#1142),#915,.F.);
#3605=ADVANCED_FACE('',(#1143),#916,.T.);
#3606=ADVANCED_FACE('',(#1144,#136,#137,#138,#139,#140),#428,.T.);
#3607=ADVANCED_FACE('',(#1145,#141,#142,#143,#144,#145),#429,.F.);
#3608=ADVANCED_FACE('',(#1146,#146),#430,.T.);
#3609=ADVANCED_FACE('',(#1147),#431,.F.);
#3610=ADVANCED_FACE('',(#1148),#432,.F.);
#3611=ADVANCED_FACE('',(#1149),#433,.F.);
#3612=ADVANCED_FACE('',(#1150),#434,.F.);
#3613=ADVANCED_FACE('',(#1151),#435,.F.);
#3614=ADVANCED_FACE('',(#1152),#436,.T.);
#3615=ADVANCED_FACE('',(#1153),#917,.T.);
#3616=ADVANCED_FACE('',(#1154),#116,.T.);
#3617=ADVANCED_FACE('',(#1155),#117,.T.);
#3618=ADVANCED_FACE('',(#1156),#918,.T.);
#3619=ADVANCED_FACE('',(#1157),#919,.T.);
#3620=ADVANCED_FACE('',(#1158),#920,.T.);
#3621=ADVANCED_FACE('',(#1159),#921,.T.);
#3622=ADVANCED_FACE('',(#1160),#922,.T.);
#3623=ADVANCED_FACE('',(#1161),#923,.T.);
#3624=ADVANCED_FACE('',(#1162),#118,.T.);
#3625=ADVANCED_FACE('',(#1163),#119,.T.);
#3626=ADVANCED_FACE('',(#1164),#120,.T.);
#3627=ADVANCED_FACE('',(#1165),#121,.T.);
#3628=ADVANCED_FACE('',(#1166),#924,.T.);
#3629=ADVANCED_FACE('',(#1167),#925,.T.);
#3630=ADVANCED_FACE('',(#1168),#926,.T.);
#3631=ADVANCED_FACE('',(#1169),#927,.T.);
#3632=ADVANCED_FACE('',(#1170),#122,.T.);
#3633=ADVANCED_FACE('',(#1171),#123,.T.);
#3634=ADVANCED_FACE('',(#1172),#928,.T.);
#3635=ADVANCED_FACE('',(#1173),#929,.T.);
#3636=ADVANCED_FACE('',(#1174),#437,.T.);
#3637=ADVANCED_FACE('',(#1175),#438,.F.);
#3638=ADVANCED_FACE('',(#1176),#115,.F.);
#3639=ADVANCED_FACE('',(#1177),#930,.F.);
#3640=ADVANCED_FACE('',(#1178),#931,.T.);
#3641=ADVANCED_FACE('',(#1179),#439,.F.);
#3642=ADVANCED_FACE('',(#1180),#440,.F.);
#3643=ADVANCED_FACE('',(#1181),#441,.T.);
#3644=ADVANCED_FACE('',(#1182),#442,.F.);
#3645=ADVANCED_FACE('',(#1183),#443,.F.);
#3646=ADVANCED_FACE('',(#1184),#444,.F.);
#3647=ADVANCED_FACE('',(#1185),#445,.F.);
#3648=ADVANCED_FACE('',(#1186),#446,.F.);
#3649=ADVANCED_FACE('',(#1187),#3441,.F.);
#3650=ADVANCED_FACE('',(#1188),#447,.T.);
#3651=CLOSED_SHELL('',(#3442));
#3652=CLOSED_SHELL('',(#3443,#3444,#3445));
#3653=CLOSED_SHELL('',(#3446,#3447,#3448));
#3654=CLOSED_SHELL('',(#3449,#3450,#3451,#3452,#3453,#3454,#3455,#3456,
#3457,#3458,#3459,#3460,#3461,#3462,#3463,#3464,#3465,#3466,#3467,#3468,
#3469,#3470,#3471,#3472,#3473,#3474,#3475,#3476,#3477,#3478,#3479,#3480,
#3481,#3482,#3483,#3484,#3485,#3486,#3487,#3488,#3489,#3490,#3491,#3492,
#3493,#3494,#3495,#3496,#3497,#3498,#3499,#3500,#3501,#3502,#3503,#3504,
#3505,#3506,#3507,#3508,#3509,#3510,#3511,#3512,#3513,#3514,#3515,#3516,
#3517,#3518,#3519,#3520,#3521,#3522,#3523,#3524,#3525,#3526,#3527,#3528,
#3529,#3530,#3531,#3532,#3533,#3534,#3535,#3536,#3537,#3538,#3539,#3540,
#3541,#3542,#3543,#3544,#3545,#3546,#3547,#3548,#3549,#3550,#3551,#3552,
#3553,#3554,#3555,#3556,#3557,#3558,#3559,#3560,#3561,#3562,#3563,#3564));
#3655=CLOSED_SHELL('',(#3565,#3566,#3567,#3568,#3569,#3570,#3571,#3572,
#3573,#3574,#3575,#3576,#3577,#3578,#3579,#3580,#3581,#3582,#3583,#3584,
#3585,#3586,#3587));
#3656=CLOSED_SHELL('',(#3588,#3589,#3590));
#3657=CLOSED_SHELL('',(#3591,#3592,#3593,#3594));
#3658=CLOSED_SHELL('',(#3595,#3596,#3597,#3598));
#3659=CLOSED_SHELL('',(#3599,#3600,#3601,#3602,#3603,#3604,#3605,#3606,
#3607,#3608));
#3660=CLOSED_SHELL('',(#3609,#3610,#3611,#3612,#3613,#3614,#3615,#3616,
#3617,#3618,#3619,#3620,#3621,#3622,#3623,#3624,#3625,#3626,#3627,#3628,
#3629,#3630,#3631,#3632,#3633,#3634));
#3661=CLOSED_SHELL('',(#3635,#3636,#3637));
#3662=CLOSED_SHELL('',(#3638,#3639,#3640,#3641,#3642,#3643,#3644,#3645,
#3646,#3647,#3648,#3649,#3650));
#3663=DERIVED_UNIT_ELEMENT(#3687,1.);
#3664=DERIVED_UNIT_ELEMENT(#20660,-3.);
#3665=DERIVED_UNIT_ELEMENT(#3687,1.);
#3666=DERIVED_UNIT_ELEMENT(#20660,-3.);
#3667=DERIVED_UNIT_ELEMENT(#3687,1.);
#3668=DERIVED_UNIT_ELEMENT(#20660,-3.);
#3669=DERIVED_UNIT_ELEMENT(#3687,1.);
#3670=DERIVED_UNIT_ELEMENT(#20660,-3.);
#3671=DERIVED_UNIT_ELEMENT(#3687,1.);
#3672=DERIVED_UNIT_ELEMENT(#20660,-3.);
#3673=DERIVED_UNIT_ELEMENT(#3687,1.);
#3674=DERIVED_UNIT_ELEMENT(#20660,-3.);
#3675=DERIVED_UNIT_ELEMENT(#3687,1.);
#3676=DERIVED_UNIT_ELEMENT(#20660,-3.);
#3677=DERIVED_UNIT_ELEMENT(#3687,1.);
#3678=DERIVED_UNIT_ELEMENT(#20660,-3.);
#3679=DERIVED_UNIT_ELEMENT(#3687,1.);
#3680=DERIVED_UNIT_ELEMENT(#20660,-3.);
#3681=DERIVED_UNIT_ELEMENT(#3687,1.);
#3682=DERIVED_UNIT_ELEMENT(#20660,-3.);
#3683=DERIVED_UNIT_ELEMENT(#3687,1.);
#3684=DERIVED_UNIT_ELEMENT(#20660,-3.);
#3685=DERIVED_UNIT_ELEMENT(#3687,1.);
#3686=DERIVED_UNIT_ELEMENT(#20660,-3.);
#3687=(
MASS_UNIT()
NAMED_UNIT(*)
SI_UNIT(.KILO.,.GRAM.)
);
#3688=DERIVED_UNIT((#3663,#3664));
#3689=DERIVED_UNIT((#3665,#3666));
#3690=DERIVED_UNIT((#3667,#3668));
#3691=DERIVED_UNIT((#3669,#3670));
#3692=DERIVED_UNIT((#3671,#3672));
#3693=DERIVED_UNIT((#3673,#3674));
#3694=DERIVED_UNIT((#3675,#3676));
#3695=DERIVED_UNIT((#3677,#3678));
#3696=DERIVED_UNIT((#3679,#3680));
#3697=DERIVED_UNIT((#3681,#3682));
#3698=DERIVED_UNIT((#3683,#3684));
#3699=DERIVED_UNIT((#3685,#3686));
#3700=MEASURE_REPRESENTATION_ITEM('density measure',
POSITIVE_RATIO_MEASURE(7850.),#3688);
#3701=MEASURE_REPRESENTATION_ITEM('density measure',
POSITIVE_RATIO_MEASURE(7850.),#3689);
#3702=MEASURE_REPRESENTATION_ITEM('density measure',
POSITIVE_RATIO_MEASURE(7850.),#3690);
#3703=MEASURE_REPRESENTATION_ITEM('density measure',
POSITIVE_RATIO_MEASURE(7850.),#3691);
#3704=MEASURE_REPRESENTATION_ITEM('density measure',
POSITIVE_RATIO_MEASURE(7850.),#3692);
#3705=MEASURE_REPRESENTATION_ITEM('density measure',
POSITIVE_RATIO_MEASURE(7850.),#3693);
#3706=MEASURE_REPRESENTATION_ITEM('density measure',
POSITIVE_RATIO_MEASURE(7850.),#3694);
#3707=MEASURE_REPRESENTATION_ITEM('density measure',
POSITIVE_RATIO_MEASURE(7850.),#3695);
#3708=MEASURE_REPRESENTATION_ITEM('density measure',
POSITIVE_RATIO_MEASURE(7850.),#3696);
#3709=MEASURE_REPRESENTATION_ITEM('density measure',
POSITIVE_RATIO_MEASURE(7850.),#3697);
#3710=MEASURE_REPRESENTATION_ITEM('density measure',
POSITIVE_RATIO_MEASURE(7850.),#3698);
#3711=MEASURE_REPRESENTATION_ITEM('density measure',
POSITIVE_RATIO_MEASURE(7850.),#3699);
#3712=PROPERTY_DEFINITION_REPRESENTATION(#3772,#3736);
#3713=PROPERTY_DEFINITION_REPRESENTATION(#3773,#3737);
#3714=PROPERTY_DEFINITION_REPRESENTATION(#3774,#3738);
#3715=PROPERTY_DEFINITION_REPRESENTATION(#3775,#3739);
#3716=PROPERTY_DEFINITION_REPRESENTATION(#3776,#3740);
#3717=PROPERTY_DEFINITION_REPRESENTATION(#3777,#3741);
#3718=PROPERTY_DEFINITION_REPRESENTATION(#3778,#3742);
#3719=PROPERTY_DEFINITION_REPRESENTATION(#3779,#3743);
#3720=PROPERTY_DEFINITION_REPRESENTATION(#3780,#3744);
#3721=PROPERTY_DEFINITION_REPRESENTATION(#3781,#3745);
#3722=PROPERTY_DEFINITION_REPRESENTATION(#3782,#3746);
#3723=PROPERTY_DEFINITION_REPRESENTATION(#3783,#3747);
#3724=PROPERTY_DEFINITION_REPRESENTATION(#3784,#3748);
#3725=PROPERTY_DEFINITION_REPRESENTATION(#3785,#3749);
#3726=PROPERTY_DEFINITION_REPRESENTATION(#3786,#3750);
#3727=PROPERTY_DEFINITION_REPRESENTATION(#3787,#3751);
#3728=PROPERTY_DEFINITION_REPRESENTATION(#3788,#3752);
#3729=PROPERTY_DEFINITION_REPRESENTATION(#3789,#3753);
#3730=PROPERTY_DEFINITION_REPRESENTATION(#3790,#3754);
#3731=PROPERTY_DEFINITION_REPRESENTATION(#3791,#3755);
#3732=PROPERTY_DEFINITION_REPRESENTATION(#3792,#3756);
#3733=PROPERTY_DEFINITION_REPRESENTATION(#3793,#3757);
#3734=PROPERTY_DEFINITION_REPRESENTATION(#3794,#3758);
#3735=PROPERTY_DEFINITION_REPRESENTATION(#3795,#3759);
#3736=REPRESENTATION('material name',(#3760),#20646);
#3737=REPRESENTATION('density',(#3700),#20646);
#3738=REPRESENTATION('material name',(#3761),#20647);
#3739=REPRESENTATION('density',(#3701),#20647);
#3740=REPRESENTATION('material name',(#3762),#20648);
#3741=REPRESENTATION('density',(#3702),#20648);
#3742=REPRESENTATION('material name',(#3763),#20649);
#3743=REPRESENTATION('density',(#3703),#20649);
#3744=REPRESENTATION('material name',(#3764),#20650);
#3745=REPRESENTATION('density',(#3704),#20650);
#3746=REPRESENTATION('material name',(#3765),#20651);
#3747=REPRESENTATION('density',(#3705),#20651);
#3748=REPRESENTATION('material name',(#3766),#20652);
#3749=REPRESENTATION('density',(#3706),#20652);
#3750=REPRESENTATION('material name',(#3767),#20653);
#3751=REPRESENTATION('density',(#3707),#20653);
#3752=REPRESENTATION('material name',(#3768),#20654);
#3753=REPRESENTATION('density',(#3708),#20654);
#3754=REPRESENTATION('material name',(#3769),#20655);
#3755=REPRESENTATION('density',(#3709),#20655);
#3756=REPRESENTATION('material name',(#3770),#20656);
#3757=REPRESENTATION('density',(#3710),#20656);
#3758=REPRESENTATION('material name',(#3771),#20657);
#3759=REPRESENTATION('density',(#3711),#20657);
#3760=DESCRIPTIVE_REPRESENTATION_ITEM('Steel','Steel');
#3761=DESCRIPTIVE_REPRESENTATION_ITEM('Steel','Steel');
#3762=DESCRIPTIVE_REPRESENTATION_ITEM('Steel','Steel');
#3763=DESCRIPTIVE_REPRESENTATION_ITEM('Steel','Steel');
#3764=DESCRIPTIVE_REPRESENTATION_ITEM('Steel','Steel');
#3765=DESCRIPTIVE_REPRESENTATION_ITEM('Steel','Steel');
#3766=DESCRIPTIVE_REPRESENTATION_ITEM('Steel','Steel');
#3767=DESCRIPTIVE_REPRESENTATION_ITEM('Steel','Steel');
#3768=DESCRIPTIVE_REPRESENTATION_ITEM('Steel','Steel');
#3769=DESCRIPTIVE_REPRESENTATION_ITEM('Steel','Steel');
#3770=DESCRIPTIVE_REPRESENTATION_ITEM('Steel','Steel');
#3771=DESCRIPTIVE_REPRESENTATION_ITEM('Steel','Steel');
#3772=PROPERTY_DEFINITION('material property','material name',#20730);
#3773=PROPERTY_DEFINITION('material property','density of part',#20730);
#3774=PROPERTY_DEFINITION('material property','material name',#20731);
#3775=PROPERTY_DEFINITION('material property','density of part',#20731);
#3776=PROPERTY_DEFINITION('material property','material name',#20732);
#3777=PROPERTY_DEFINITION('material property','density of part',#20732);
#3778=PROPERTY_DEFINITION('material property','material name',#20733);
#3779=PROPERTY_DEFINITION('material property','density of part',#20733);
#3780=PROPERTY_DEFINITION('material property','material name',#20734);
#3781=PROPERTY_DEFINITION('material property','density of part',#20734);
#3782=PROPERTY_DEFINITION('material property','material name',#20735);
#3783=PROPERTY_DEFINITION('material property','density of part',#20735);
#3784=PROPERTY_DEFINITION('material property','material name',#20736);
#3785=PROPERTY_DEFINITION('material property','density of part',#20736);
#3786=PROPERTY_DEFINITION('material property','material name',#20737);
#3787=PROPERTY_DEFINITION('material property','density of part',#20737);
#3788=PROPERTY_DEFINITION('material property','material name',#20738);
#3789=PROPERTY_DEFINITION('material property','density of part',#20738);
#3790=PROPERTY_DEFINITION('material property','material name',#20739);
#3791=PROPERTY_DEFINITION('material property','density of part',#20739);
#3792=PROPERTY_DEFINITION('material property','material name',#20740);
#3793=PROPERTY_DEFINITION('material property','density of part',#20740);
#3794=PROPERTY_DEFINITION('material property','material name',#20741);
#3795=PROPERTY_DEFINITION('material property','density of part',#20741);
#3796=AXIS2_PLACEMENT_3D('',#4988,#4129,#4130);
#3797=AXIS2_PLACEMENT_3D('',#4989,#4131,#4132);
#3798=AXIS2_PLACEMENT_3D('',#4990,#4133,#4134);
#3799=AXIS2_PLACEMENT_3D('',#4992,#4135,#4136);
#3800=AXIS2_PLACEMENT_3D('',#4993,#4137,#4138);
#3801=AXIS2_PLACEMENT_3D('',#4994,#4139,#4140);
#3802=AXIS2_PLACEMENT_3D('',#4995,#4141,#4142);
#3803=AXIS2_PLACEMENT_3D('',#4997,#4143,#4144);
#3804=AXIS2_PLACEMENT_3D('',#5000,#4146,#4147);
#3805=AXIS2_PLACEMENT_3D('',#5001,#4148,#4149);
#3806=AXIS2_PLACEMENT_3D('',#5002,#4150,#4151);
#3807=AXIS2_PLACEMENT_3D('',#5003,#4152,#4153);
#3808=AXIS2_PLACEMENT_3D('',#5004,#4154,#4155);
#3809=AXIS2_PLACEMENT_3D('',#5006,#4156,#4157);
#3810=AXIS2_PLACEMENT_3D('',#5009,#4159,#4160);
#3811=AXIS2_PLACEMENT_3D('',#5010,#4161,#4162);
#3812=AXIS2_PLACEMENT_3D('',#5011,#4163,#4164);
#3813=AXIS2_PLACEMENT_3D('',#5012,#4165,#4166);
#3814=AXIS2_PLACEMENT_3D('',#5013,#4167,#4168);
#3815=AXIS2_PLACEMENT_3D('',#5015,#4169,#4170);
#3816=AXIS2_PLACEMENT_3D('',#5018,#4172,#4173);
#3817=AXIS2_PLACEMENT_3D('',#5019,#4174,#4175);
#3818=AXIS2_PLACEMENT_3D('',#5021,#4176,#4177);
#3819=AXIS2_PLACEMENT_3D('',#5024,#4179,#4180);
#3820=AXIS2_PLACEMENT_3D('',#5025,#4181,#4182);
#3821=AXIS2_PLACEMENT_3D('',#5028,#4183,#4184);
#3822=AXIS2_PLACEMENT_3D('',#5045,#4185,#4186);
#3823=AXIS2_PLACEMENT_3D('',#5048,#4188,#4189);
#3824=AXIS2_PLACEMENT_3D('',#5050,#4190,#4191);
#3825=AXIS2_PLACEMENT_3D('',#5065,#4192,#4193);
#3826=AXIS2_PLACEMENT_3D('',#5087,#4194,#4195);
#3827=AXIS2_PLACEMENT_3D('',#5089,#4196,#4197);
#3828=AXIS2_PLACEMENT_3D('',#5098,#4199,#4200);
#3829=AXIS2_PLACEMENT_3D('',#5122,#4202,#4203);
#3830=AXIS2_PLACEMENT_3D('',#5147,#4206,#4207);
#3831=AXIS2_PLACEMENT_3D('',#5165,#4210,#4211);
#3832=AXIS2_PLACEMENT_3D('',#5180,#4213,#4214);
#3833=AXIS2_PLACEMENT_3D('',#5205,#4217,#4218);
#3834=AXIS2_PLACEMENT_3D('',#5207,#4220,#4221);
#3835=AXIS2_PLACEMENT_3D('',#5228,#4224,#4225);
#3836=AXIS2_PLACEMENT_3D('',#5252,#4227,#4228);
#3837=AXIS2_PLACEMENT_3D('',#5273,#4231,#4232);
#3838=AXIS2_PLACEMENT_3D('',#5294,#4235,#4236);
#3839=AXIS2_PLACEMENT_3D('',#5315,#4239,#4240);
#3840=AXIS2_PLACEMENT_3D('',#5336,#4243,#4244);
#3841=AXIS2_PLACEMENT_3D('',#5357,#4247,#4248);
#3842=AXIS2_PLACEMENT_3D('',#5378,#4251,#4252);
#3843=AXIS2_PLACEMENT_3D('',#5399,#4255,#4256);
#3844=AXIS2_PLACEMENT_3D('',#5413,#4259,#4260);
#3845=AXIS2_PLACEMENT_3D('',#5414,#4261,#4262);
#3846=AXIS2_PLACEMENT_3D('',#5435,#4265,#4266);
#3847=AXIS2_PLACEMENT_3D('',#5456,#4269,#4270);
#3848=AXIS2_PLACEMENT_3D('',#5477,#4273,#4274);
#3849=AXIS2_PLACEMENT_3D('',#5498,#4277,#4278);
#3850=AXIS2_PLACEMENT_3D('',#5519,#4281,#4282);
#3851=AXIS2_PLACEMENT_3D('',#5839,#4285,#4286);
#3852=AXIS2_PLACEMENT_3D('',#6461,#4287,#4288);
#3853=AXIS2_PLACEMENT_3D('',#7083,#4289,#4290);
#3854=AXIS2_PLACEMENT_3D('',#7705,#4291,#4292);
#3855=AXIS2_PLACEMENT_3D('',#8330,#4294,#4295);
#3856=AXIS2_PLACEMENT_3D('',#8332,#4296,#4297);
#3857=AXIS2_PLACEMENT_3D('',#8343,#4299,#4300);
#3858=AXIS2_PLACEMENT_3D('',#8650,#4301,#4302);
#3859=AXIS2_PLACEMENT_3D('',#9272,#4303,#4304);
#3860=AXIS2_PLACEMENT_3D('',#9894,#4305,#4306);
#3861=AXIS2_PLACEMENT_3D('',#10849,#4307,#4308);
#3862=AXIS2_PLACEMENT_3D('',#10856,#4309,#4310);
#3863=AXIS2_PLACEMENT_3D('',#10868,#4313,#4314);
#3864=AXIS2_PLACEMENT_3D('',#10880,#4317,#4318);
#3865=AXIS2_PLACEMENT_3D('',#10892,#4321,#4322);
#3866=AXIS2_PLACEMENT_3D('',#10904,#4325,#4326);
#3867=AXIS2_PLACEMENT_3D('',#10916,#4329,#4330);
#3868=AXIS2_PLACEMENT_3D('',#10928,#4333,#4334);
#3869=AXIS2_PLACEMENT_3D('',#10940,#4337,#4338);
#3870=AXIS2_PLACEMENT_3D('',#10952,#4341,#4342);
#3871=AXIS2_PLACEMENT_3D('',#10964,#4345,#4346);
#3872=AXIS2_PLACEMENT_3D('',#10976,#4349,#4350);
#3873=AXIS2_PLACEMENT_3D('',#10988,#4353,#4354);
#3874=AXIS2_PLACEMENT_3D('',#11000,#4357,#4358);
#3875=AXIS2_PLACEMENT_3D('',#11012,#4361,#4362);
#3876=AXIS2_PLACEMENT_3D('',#11024,#4365,#4366);
#3877=AXIS2_PLACEMENT_3D('',#11036,#4369,#4370);
#3878=AXIS2_PLACEMENT_3D('',#11053,#4373,#4374);
#3879=AXIS2_PLACEMENT_3D('',#11065,#4377,#4378);
#3880=AXIS2_PLACEMENT_3D('',#11091,#4381,#4382);
#3881=AXIS2_PLACEMENT_3D('',#11429,#4385,#4386);
#3882=AXIS2_PLACEMENT_3D('',#14177,#4389,#4390);
#3883=AXIS2_PLACEMENT_3D('',#14482,#4391,#4392);
#3884=AXIS2_PLACEMENT_3D('',#14773,#4393,#4394);
#3885=AXIS2_PLACEMENT_3D('',#15078,#4395,#4396);
#3886=AXIS2_PLACEMENT_3D('',#15369,#4397,#4398);
#3887=AXIS2_PLACEMENT_3D('',#15674,#4399,#4400);
#3888=AXIS2_PLACEMENT_3D('',#15965,#4401,#4402);
#3889=AXIS2_PLACEMENT_3D('',#16270,#4403,#4404);
#3890=AXIS2_PLACEMENT_3D('',#16882,#4405,#4406);
#3891=AXIS2_PLACEMENT_3D('',#16885,#4408,#4409);
#3892=AXIS2_PLACEMENT_3D('',#16887,#4411,#4412);
#3893=AXIS2_PLACEMENT_3D('',#16890,#4414,#4415);
#3894=AXIS2_PLACEMENT_3D('',#16892,#4417,#4418);
#3895=AXIS2_PLACEMENT_3D('',#16896,#4421,#4422);
#3896=AXIS2_PLACEMENT_3D('',#16897,#4423,#4424);
#3897=AXIS2_PLACEMENT_3D('',#16900,#4427,#4428);
#3898=AXIS2_PLACEMENT_3D('',#16903,#4431,#4432);
#3899=AXIS2_PLACEMENT_3D('',#16936,#4435,#4436);
#3900=AXIS2_PLACEMENT_3D('',#16972,#4438,#4439);
#3901=AXIS2_PLACEMENT_3D('',#16996,#4441,#4442);
#3902=AXIS2_PLACEMENT_3D('',#17301,#4444,#4445);
#3903=AXIS2_PLACEMENT_3D('',#18306,#4448,#4449);
#3904=AXIS2_PLACEMENT_3D('',#18307,#4450,#4451);
#3905=AXIS2_PLACEMENT_3D('',#18324,#4453,#4454);
#3906=AXIS2_PLACEMENT_3D('',#18342,#4457,#4458);
#3907=AXIS2_PLACEMENT_3D('',#18366,#4460,#4461);
#3908=AXIS2_PLACEMENT_3D('',#18664,#4462,#4463);
#3909=AXIS2_PLACEMENT_3D('',#19313,#4465,#4466);
#3910=AXIS2_PLACEMENT_3D('',#19318,#4471,#4472);
#3911=AXIS2_PLACEMENT_3D('',#19322,#4475,#4476);
#3912=AXIS2_PLACEMENT_3D('',#19325,#4479,#4480);
#3913=AXIS2_PLACEMENT_3D('',#19327,#4482,#4483);
#3914=AXIS2_PLACEMENT_3D('',#19329,#4485,#4486);
#3915=AXIS2_PLACEMENT_3D('',#19332,#4489,#4490);
#3916=AXIS2_PLACEMENT_3D('',#19333,#4491,#4492);
#3917=AXIS2_PLACEMENT_3D('',#19334,#4493,#4494);
#3918=AXIS2_PLACEMENT_3D('',#19335,#4495,#4496);
#3919=AXIS2_PLACEMENT_3D('',#19336,#4497,#4498);
#3920=AXIS2_PLACEMENT_3D('',#19337,#4499,#4500);
#3921=AXIS2_PLACEMENT_3D('',#19338,#4501,#4502);
#3922=AXIS2_PLACEMENT_3D('',#19341,#4505,#4506);
#3923=AXIS2_PLACEMENT_3D('',#19342,#4507,#4508);
#3924=AXIS2_PLACEMENT_3D('',#19343,#4509,#4510);
#3925=AXIS2_PLACEMENT_3D('',#19344,#4511,#4512);
#3926=AXIS2_PLACEMENT_3D('',#19345,#4513,#4514);
#3927=AXIS2_PLACEMENT_3D('',#19346,#4515,#4516);
#3928=AXIS2_PLACEMENT_3D('',#19347,#4517,#4518);
#3929=AXIS2_PLACEMENT_3D('',#19348,#4519,#4520);
#3930=AXIS2_PLACEMENT_3D('',#19349,#4521,#4522);
#3931=AXIS2_PLACEMENT_3D('',#19350,#4523,#4524);
#3932=AXIS2_PLACEMENT_3D('',#19351,#4525,#4526);
#3933=AXIS2_PLACEMENT_3D('',#19352,#4527,#4528);
#3934=AXIS2_PLACEMENT_3D('',#19361,#4530,#4531);
#3935=AXIS2_PLACEMENT_3D('',#19373,#4533,#4534);
#3936=AXIS2_PLACEMENT_3D('',#19427,#4536,#4537);
#3937=AXIS2_PLACEMENT_3D('',#19481,#4539,#4540);
#3938=AXIS2_PLACEMENT_3D('',#19514,#4543,#4544);
#3939=AXIS2_PLACEMENT_3D('',#19519,#4546,#4547);
#3940=AXIS2_PLACEMENT_3D('',#19548,#4548,#4549);
#3941=AXIS2_PLACEMENT_3D('',#19582,#4552,#4553);
#3942=AXIS2_PLACEMENT_3D('',#19619,#4554,#4555);
#3943=AXIS2_PLACEMENT_3D('',#19699,#4557,#4558);
#3944=AXIS2_PLACEMENT_3D('',#19725,#4561,#4562);
#3945=AXIS2_PLACEMENT_3D('',#19746,#4563,#4564);
#3946=AXIS2_PLACEMENT_3D('',#19748,#4565,#4566);
#3947=AXIS2_PLACEMENT_3D('',#19751,#4568,#4569);
#3948=AXIS2_PLACEMENT_3D('',#19752,#4570,#4571);
#3949=AXIS2_PLACEMENT_3D('',#19754,#4572,#4573);
#3950=AXIS2_PLACEMENT_3D('',#19757,#4575,#4576);
#3951=AXIS2_PLACEMENT_3D('',#19758,#4577,#4578);
#3952=AXIS2_PLACEMENT_3D('',#19760,#4579,#4580);
#3953=AXIS2_PLACEMENT_3D('',#19763,#4582,#4583);
#3954=AXIS2_PLACEMENT_3D('',#19764,#4584,#4585);
#3955=AXIS2_PLACEMENT_3D('',#19766,#4586,#4587);
#3956=AXIS2_PLACEMENT_3D('',#19769,#4589,#4590);
#3957=AXIS2_PLACEMENT_3D('',#19770,#4591,#4592);
#3958=AXIS2_PLACEMENT_3D('',#19843,#4593,#4594);
#3959=AXIS2_PLACEMENT_3D('',#19846,#4597,#4598);
#3960=AXIS2_PLACEMENT_3D('',#20102,#4600,#4601);
#3961=AXIS2_PLACEMENT_3D('',#20103,#4602,#4603);
#3962=AXIS2_PLACEMENT_3D('',#20104,#4604,#4605);
#3963=AXIS2_PLACEMENT_3D('',#20296,#4607,#4608);
#3964=AXIS2_PLACEMENT_3D('',#20297,#4609,#4610);
#3965=AXIS2_PLACEMENT_3D('',#20298,#4611,#4612);
#3966=AXIS2_PLACEMENT_3D('',#20299,#4613,#4614);
#3967=AXIS2_PLACEMENT_3D('',#20300,#4615,#4616);
#3968=AXIS2_PLACEMENT_3D('',#20302,#4617,#4618);
#3969=AXIS2_PLACEMENT_3D('',#20305,#4620,#4621);
#3970=AXIS2_PLACEMENT_3D('',#20306,#4622,#4623);
#3971=AXIS2_PLACEMENT_3D('',#20307,#4624,#4625);
#3972=AXIS2_PLACEMENT_3D('',#20308,#4626,#4627);
#3973=AXIS2_PLACEMENT_3D('',#20309,#4628,#4629);
#3974=AXIS2_PLACEMENT_3D('',#20311,#4630,#4631);
#3975=AXIS2_PLACEMENT_3D('',#20314,#4633,#4634);
#3976=AXIS2_PLACEMENT_3D('',#20315,#4635,#4636);
#3977=AXIS2_PLACEMENT_3D('',#20317,#4637,#4638);
#3978=AXIS2_PLACEMENT_3D('',#20320,#4640,#4641);
#3979=AXIS2_PLACEMENT_3D('',#20321,#4642,#4643);
#3980=AXIS2_PLACEMENT_3D('',#20322,#4644,#4645);
#3981=AXIS2_PLACEMENT_3D('',#20323,#4646,#4647);
#3982=AXIS2_PLACEMENT_3D('',#20324,#4648,#4649);
#3983=AXIS2_PLACEMENT_3D('',#20326,#4650,#4651);
#3984=AXIS2_PLACEMENT_3D('',#20329,#4653,#4654);
#3985=AXIS2_PLACEMENT_3D('',#20330,#4655,#4656);
#3986=AXIS2_PLACEMENT_3D('',#20332,#4657,#4658);
#3987=AXIS2_PLACEMENT_3D('',#20335,#4660,#4661);
#3988=AXIS2_PLACEMENT_3D('',#20336,#4662,#4663);
#3989=AXIS2_PLACEMENT_3D('',#20337,#4664,#4665);
#3990=AXIS2_PLACEMENT_3D('',#20338,#4666,#4667);
#3991=AXIS2_PLACEMENT_3D('',#20339,#4668,#4669);
#3992=AXIS2_PLACEMENT_3D('',#20341,#4670,#4671);
#3993=AXIS2_PLACEMENT_3D('',#20344,#4673,#4674);
#3994=AXIS2_PLACEMENT_3D('',#20345,#4675,#4676);
#3995=AXIS2_PLACEMENT_3D('',#20347,#4677,#4678);
#3996=AXIS2_PLACEMENT_3D('',#20350,#4680,#4681);
#3997=AXIS2_PLACEMENT_3D('',#20351,#4682,#4683);
#3998=AXIS2_PLACEMENT_3D('',#20353,#4684,#4685);
#3999=AXIS2_PLACEMENT_3D('',#20356,#4687,#4688);
#4000=AXIS2_PLACEMENT_3D('',#20357,#4689,#4690);
#4001=AXIS2_PLACEMENT_3D('',#20359,#4691,#4692);
#4002=AXIS2_PLACEMENT_3D('',#20362,#4694,#4695);
#4003=AXIS2_PLACEMENT_3D('',#20363,#4696,#4697);
#4004=AXIS2_PLACEMENT_3D('',#20365,#4698,#4699);
#4005=AXIS2_PLACEMENT_3D('',#20368,#4701,#4702);
#4006=AXIS2_PLACEMENT_3D('',#20369,#4703,#4704);
#4007=AXIS2_PLACEMENT_3D('',#20371,#4705,#4706);
#4008=AXIS2_PLACEMENT_3D('',#20374,#4708,#4709);
#4009=AXIS2_PLACEMENT_3D('',#20375,#4710,#4711);
#4010=AXIS2_PLACEMENT_3D('',#20377,#4712,#4713);
#4011=AXIS2_PLACEMENT_3D('',#20380,#4715,#4716);
#4012=AXIS2_PLACEMENT_3D('',#20381,#4717,#4718);
#4013=AXIS2_PLACEMENT_3D('',#20382,#4719,#4720);
#4014=AXIS2_PLACEMENT_3D('',#20383,#4721,#4722);
#4015=AXIS2_PLACEMENT_3D('',#20384,#4723,#4724);
#4016=AXIS2_PLACEMENT_3D('',#20385,#4725,#4726);
#4017=AXIS2_PLACEMENT_3D('',#20394,#4731,#4732);
#4018=AXIS2_PLACEMENT_3D('',#20403,#4737,#4738);
#4019=AXIS2_PLACEMENT_3D('',#20412,#4743,#4744);
#4020=AXIS2_PLACEMENT_3D('',#20421,#4749,#4750);
#4021=AXIS2_PLACEMENT_3D('',#20430,#4755,#4756);
#4022=AXIS2_PLACEMENT_3D('',#20439,#4761,#4762);
#4023=AXIS2_PLACEMENT_3D('',#20440,#4763,#4764);
#4024=AXIS2_PLACEMENT_3D('',#20441,#4765,#4766);
#4025=AXIS2_PLACEMENT_3D('',#20442,#4767,#4768);
#4026=AXIS2_PLACEMENT_3D('',#20443,#4769,#4770);
#4027=AXIS2_PLACEMENT_3D('',#20444,#4771,#4772);
#4028=AXIS2_PLACEMENT_3D('',#20445,#4773,#4774);
#4029=AXIS2_PLACEMENT_3D('',#20446,#4775,#4776);
#4030=AXIS2_PLACEMENT_3D('',#20447,#4777,#4778);
#4031=AXIS2_PLACEMENT_3D('',#20448,#4779,#4780);
#4032=AXIS2_PLACEMENT_3D('',#20449,#4781,#4782);
#4033=AXIS2_PLACEMENT_3D('',#20450,#4783,#4784);
#4034=AXIS2_PLACEMENT_3D('',#20451,#4785,#4786);
#4035=AXIS2_PLACEMENT_3D('',#20452,#4787,#4788);
#4036=AXIS2_PLACEMENT_3D('',#20453,#4789,#4790);
#4037=AXIS2_PLACEMENT_3D('',#20454,#4791,#4792);
#4038=AXIS2_PLACEMENT_3D('',#20455,#4793,#4794);
#4039=AXIS2_PLACEMENT_3D('',#20456,#4795,#4796);
#4040=AXIS2_PLACEMENT_3D('',#20457,#4797,#4798);
#4041=AXIS2_PLACEMENT_3D('',#20458,#4799,#4800);
#4042=AXIS2_PLACEMENT_3D('',#20459,#4801,#4802);
#4043=AXIS2_PLACEMENT_3D('',#20460,#4803,#4804);
#4044=AXIS2_PLACEMENT_3D('',#20461,#4805,#4806);
#4045=AXIS2_PLACEMENT_3D('',#20462,#4807,#4808);
#4046=AXIS2_PLACEMENT_3D('',#20463,#4809,#4810);
#4047=AXIS2_PLACEMENT_3D('',#20464,#4811,#4812);
#4048=AXIS2_PLACEMENT_3D('',#20465,#4813,#4814);
#4049=AXIS2_PLACEMENT_3D('',#20466,#4815,#4816);
#4050=AXIS2_PLACEMENT_3D('',#20467,#4817,#4818);
#4051=AXIS2_PLACEMENT_3D('',#20468,#4819,#4820);
#4052=AXIS2_PLACEMENT_3D('',#20469,#4821,#4822);
#4053=AXIS2_PLACEMENT_3D('',#20470,#4823,#4824);
#4054=AXIS2_PLACEMENT_3D('',#20471,#4825,#4826);
#4055=AXIS2_PLACEMENT_3D('',#20472,#4827,#4828);
#4056=AXIS2_PLACEMENT_3D('',#20473,#4829,#4830);
#4057=AXIS2_PLACEMENT_3D('',#20474,#4831,#4832);
#4058=AXIS2_PLACEMENT_3D('',#20475,#4833,#4834);
#4059=AXIS2_PLACEMENT_3D('',#20476,#4835,#4836);
#4060=AXIS2_PLACEMENT_3D('',#20477,#4837,#4838);
#4061=AXIS2_PLACEMENT_3D('',#20478,#4839,#4840);
#4062=AXIS2_PLACEMENT_3D('',#20479,#4841,#4842);
#4063=AXIS2_PLACEMENT_3D('',#20480,#4843,#4844);
#4064=AXIS2_PLACEMENT_3D('',#20481,#4845,#4846);
#4065=AXIS2_PLACEMENT_3D('',#20482,#4847,#4848);
#4066=AXIS2_PLACEMENT_3D('',#20483,#4849,#4850);
#4067=AXIS2_PLACEMENT_3D('',#20484,#4851,#4852);
#4068=AXIS2_PLACEMENT_3D('',#20486,#4853,#4854);
#4069=AXIS2_PLACEMENT_3D('',#20489,#4856,#4857);
#4070=AXIS2_PLACEMENT_3D('',#20490,#4858,#4859);
#4071=AXIS2_PLACEMENT_3D('',#20491,#4860,#4861);
#4072=AXIS2_PLACEMENT_3D('',#20492,#4862,#4863);
#4073=AXIS2_PLACEMENT_3D('',#20493,#4864,#4865);
#4074=AXIS2_PLACEMENT_3D('',#20496,#4866,#4867);
#4075=AXIS2_PLACEMENT_3D('',#20502,#4868,#4869);
#4076=AXIS2_PLACEMENT_3D('',#20506,#4870,#4871);
#4077=AXIS2_PLACEMENT_3D('',#20508,#4872,#4873);
#4078=AXIS2_PLACEMENT_3D('',#20512,#4875,#4876);
#4079=AXIS2_PLACEMENT_3D('',#20515,#4878,#4879);
#4080=AXIS2_PLACEMENT_3D('',#20517,#4880,#4881);
#4081=AXIS2_PLACEMENT_3D('',#20520,#4883,#4884);
#4082=AXIS2_PLACEMENT_3D('',#20521,#4885,#4886);
#4083=AXIS2_PLACEMENT_3D('',#20524,#4887,#4888);
#4084=AXIS2_PLACEMENT_3D('',#20549,#4889,#4890);
#4085=AXIS2_PLACEMENT_3D('',#20553,#4892,#4893);
#4086=AXIS2_PLACEMENT_3D('',#20555,#4894,#4895);
#4087=AXIS2_PLACEMENT_3D('',#20559,#4897,#4898);
#4088=AXIS2_PLACEMENT_3D('',#20563,#4900,#4901);
#4089=AXIS2_PLACEMENT_3D('',#20564,#4902,#4903);
#4090=AXIS2_PLACEMENT_3D('',#20566,#4904,#4905);
#4091=AXIS2_PLACEMENT_3D('',#20587,#4906,#4907);
#4092=AXIS2_PLACEMENT_3D('',#20588,#4908,#4909);
#4093=AXIS2_PLACEMENT_3D('',#20589,#4910,#4911);
#4094=AXIS2_PLACEMENT_3D('',#20590,#4912,#4913);
#4095=AXIS2_PLACEMENT_3D('',#20591,#4914,#4915);
#4096=AXIS2_PLACEMENT_3D('',#20594,#4918,#4919);
#4097=AXIS2_PLACEMENT_3D('',#20597,#4922,#4923);
#4098=AXIS2_PLACEMENT_3D('',#20599,#4925,#4926);
#4099=AXIS2_PLACEMENT_3D('',#20601,#4928,#4929);
#4100=AXIS2_PLACEMENT_3D('',#20602,#4930,#4931);
#4101=AXIS2_PLACEMENT_3D('',#20603,#4932,#4933);
#4102=AXIS2_PLACEMENT_3D('',#20604,#4934,#4935);
#4103=AXIS2_PLACEMENT_3D('',#20605,#4936,#4937);
#4104=AXIS2_PLACEMENT_3D('',#20606,#4938,#4939);
#4105=AXIS2_PLACEMENT_3D('',#20607,#4940,#4941);
#4106=AXIS2_PLACEMENT_3D('',#20608,#4942,#4943);
#4107=AXIS2_PLACEMENT_3D('',#20609,#4944,#4945);
#4108=AXIS2_PLACEMENT_3D('',#20610,#4946,#4947);
#4109=AXIS2_PLACEMENT_3D('',#20611,#4948,#4949);
#4110=AXIS2_PLACEMENT_3D('',#20612,#4950,#4951);
#4111=AXIS2_PLACEMENT_3D('',#20613,#4952,#4953);
#4112=AXIS2_PLACEMENT_3D('',#20614,#4954,#4955);
#4113=AXIS2_PLACEMENT_3D('',#20615,#4956,#4957);
#4114=AXIS2_PLACEMENT_3D('',#20616,#4958,#4959);
#4115=AXIS2_PLACEMENT_3D('',#20617,#4960,#4961);
#4116=AXIS2_PLACEMENT_3D('',#20618,#4962,#4963);
#4117=AXIS2_PLACEMENT_3D('',#20619,#4964,#4965);
#4118=AXIS2_PLACEMENT_3D('',#20620,#4966,#4967);
#4119=AXIS2_PLACEMENT_3D('',#20621,#4968,#4969);
#4120=AXIS2_PLACEMENT_3D('',#20622,#4970,#4971);
#4121=AXIS2_PLACEMENT_3D('',#20623,#4972,#4973);
#4122=AXIS2_PLACEMENT_3D('',#20624,#4974,#4975);
#4123=AXIS2_PLACEMENT_3D('',#20625,#4976,#4977);
#4124=AXIS2_PLACEMENT_3D('',#20626,#4978,#4979);
#4125=AXIS2_PLACEMENT_3D('',#20627,#4980,#4981);
#4126=AXIS2_PLACEMENT_3D('',#20628,#4982,#4983);
#4127=AXIS2_PLACEMENT_3D('',#20629,#4984,#4985);
#4128=AXIS2_PLACEMENT_3D('',#20630,#4986,#4987);
#4129=DIRECTION('axis',(0.,0.,1.));
#4130=DIRECTION('refdir',(1.,0.,0.));
#4131=DIRECTION('axis',(0.,0.,1.));
#4132=DIRECTION('refdir',(1.,0.,0.));
#4133=DIRECTION('center_axis',(0.,1.,0.));
#4134=DIRECTION('ref_axis',(0.,0.,1.));
#4135=DIRECTION('center_axis',(-1.,0.,1.15371258089726E-16));
#4136=DIRECTION('ref_axis',(-1.15371258089726E-16,0.,-1.));
#4137=DIRECTION('center_axis',(0.,-1.,0.));
#4138=DIRECTION('ref_axis',(0.,0.,1.));
#4139=DIRECTION('axis',(0.,0.,1.));
#4140=DIRECTION('refdir',(1.,0.,0.));
#4141=DIRECTION('center_axis',(-1.,0.,0.));
#4142=DIRECTION('ref_axis',(0.,0.,1.));
#4143=DIRECTION('center_axis',(1.,0.,0.));
#4144=DIRECTION('ref_axis',(0.,0.,-1.));
#4145=DIRECTION('',(1.,0.,0.));
#4146=DIRECTION('center_axis',(1.,0.,0.));
#4147=DIRECTION('ref_axis',(0.,0.,-1.));
#4148=DIRECTION('center_axis',(1.,0.,0.));
#4149=DIRECTION('ref_axis',(0.,0.,-1.));
#4150=DIRECTION('center_axis',(1.,0.,0.));
#4151=DIRECTION('ref_axis',(0.,0.,-1.));
#4152=DIRECTION('axis',(0.,0.,1.));
#4153=DIRECTION('refdir',(1.,0.,0.));
#4154=DIRECTION('center_axis',(0.,0.,-1.));
#4155=DIRECTION('ref_axis',(-1.,0.,0.));
#4156=DIRECTION('center_axis',(0.,0.,1.));
#4157=DIRECTION('ref_axis',(1.,0.,0.));
#4158=DIRECTION('',(0.,0.,1.));
#4159=DIRECTION('center_axis',(0.,0.,1.));
#4160=DIRECTION('ref_axis',(1.,0.,0.));
#4161=DIRECTION('center_axis',(0.,0.,1.));
#4162=DIRECTION('ref_axis',(1.,0.,0.));
#4163=DIRECTION('center_axis',(0.,0.,1.));
#4164=DIRECTION('ref_axis',(1.,0.,0.));
#4165=DIRECTION('axis',(0.,0.,1.));
#4166=DIRECTION('refdir',(1.,0.,0.));
#4167=DIRECTION('center_axis',(0.,-1.,0.));
#4168=DIRECTION('ref_axis',(0.,0.,-1.));
#4169=DIRECTION('center_axis',(0.,-1.,0.));
#4170=DIRECTION('ref_axis',(0.,0.,-1.));
#4171=DIRECTION('',(0.,-1.,0.));
#4172=DIRECTION('center_axis',(0.,-1.,0.));
#4173=DIRECTION('ref_axis',(0.,0.,-1.));
#4174=DIRECTION('center_axis',(0.,-1.,0.));
#4175=DIRECTION('ref_axis',(0.,0.,-1.));
#4176=DIRECTION('center_axis',(0.,1.,0.));
#4177=DIRECTION('ref_axis',(0.,0.,1.));
#4178=DIRECTION('',(0.,1.,0.));
#4179=DIRECTION('center_axis',(0.,-1.,0.));
#4180=DIRECTION('ref_axis',(0.,0.,-1.));
#4181=DIRECTION('center_axis',(0.,1.,0.));
#4182=DIRECTION('ref_axis',(0.,0.,1.));
#4183=DIRECTION('center_axis',(0.,-1.,0.));
#4184=DIRECTION('ref_axis',(0.,0.,-1.));
#4185=DIRECTION('center_axis',(0.,-1.,0.));
#4186=DIRECTION('ref_axis',(0.,0.,-1.));
#4187=DIRECTION('',(0.,-1.,0.));
#4188=DIRECTION('center_axis',(0.,-1.,0.));
#4189=DIRECTION('ref_axis',(0.,0.,-1.));
#4190=DIRECTION('center_axis',(0.,-1.,0.));
#4191=DIRECTION('ref_axis',(0.,0.,-1.));
#4192=DIRECTION('center_axis',(0.,-1.,0.));
#4193=DIRECTION('ref_axis',(0.,0.,-1.));
#4194=DIRECTION('center_axis',(0.997075912644082,0.00470397725131907,-0.0762725181372069));
#4195=DIRECTION('ref_axis',(-0.0696482235815162,-0.354761993301017,-0.932358864955457));
#4196=DIRECTION('center_axis',(0.,-1.,0.));
#4197=DIRECTION('ref_axis',(0.,0.,-1.));
#4198=DIRECTION('',(0.,-1.,0.));
#4199=DIRECTION('center_axis',(0.,-1.,0.));
#4200=DIRECTION('ref_axis',(0.,0.,-1.));
#4201=DIRECTION('',(0.,1.,0.));
#4202=DIRECTION('center_axis',(0.,1.,0.));
#4203=DIRECTION('ref_axis',(0.,0.,1.));
#4204=DIRECTION('',(0.,-1.,0.));
#4205=DIRECTION('',(0.,1.,0.));
#4206=DIRECTION('center_axis',(0.,1.,0.));
#4207=DIRECTION('ref_axis',(0.,0.,1.));
#4208=DIRECTION('',(1.10691650854818E-16,-1.,-2.86740941221399E-8));
#4209=DIRECTION('',(0.,-1.,0.));
#4210=DIRECTION('center_axis',(0.,-1.,0.));
#4211=DIRECTION('ref_axis',(0.,0.,-1.));
#4212=DIRECTION('',(0.,1.,0.));
#4213=DIRECTION('center_axis',(0.,1.,0.));
#4214=DIRECTION('ref_axis',(0.,0.,1.));
#4215=DIRECTION('',(0.,-1.,0.));
#4216=DIRECTION('',(0.,1.,0.));
#4217=DIRECTION('center_axis',(0.,1.,0.));
#4218=DIRECTION('ref_axis',(0.,0.,1.));
#4219=DIRECTION('',(0.,-1.,0.));
#4220=DIRECTION('center_axis',(0.,-1.,0.));
#4221=DIRECTION('ref_axis',(0.,0.,-1.));
#4222=DIRECTION('',(0.,1.,0.));
#4223=DIRECTION('',(0.,-1.,0.));
#4224=DIRECTION('center_axis',(0.,-1.,0.));
#4225=DIRECTION('ref_axis',(0.,0.,-1.));
#4226=DIRECTION('',(0.,-1.,0.));
#4227=DIRECTION('center_axis',(0.,-1.,0.));
#4228=DIRECTION('ref_axis',(0.,0.,-1.));
#4229=DIRECTION('',(0.,1.,0.));
#4230=DIRECTION('',(0.,-1.,0.));
#4231=DIRECTION('center_axis',(0.,-1.,0.));
#4232=DIRECTION('ref_axis',(0.,0.,-1.));
#4233=DIRECTION('',(0.,-1.,0.));
#4234=DIRECTION('',(0.,1.,0.));
#4235=DIRECTION('center_axis',(0.,-1.,0.));
#4236=DIRECTION('ref_axis',(0.,0.,-1.));
#4237=DIRECTION('',(0.,1.,0.));
#4238=DIRECTION('',(0.,-1.,0.));
#4239=DIRECTION('center_axis',(0.,-1.,0.));
#4240=DIRECTION('ref_axis',(0.,0.,-1.));
#4241=DIRECTION('',(0.,-1.,0.));
#4242=DIRECTION('',(0.,1.,0.));
#4243=DIRECTION('center_axis',(0.,-1.,0.));
#4244=DIRECTION('ref_axis',(0.,0.,-1.));
#4245=DIRECTION('',(0.,1.,0.));
#4246=DIRECTION('',(0.,-1.,0.));
#4247=DIRECTION('center_axis',(0.,-1.,0.));
#4248=DIRECTION('ref_axis',(0.,0.,-1.));
#4249=DIRECTION('',(0.,-1.,0.));
#4250=DIRECTION('',(0.,1.,0.));
#4251=DIRECTION('center_axis',(0.,-1.,0.));
#4252=DIRECTION('ref_axis',(0.,0.,-1.));
#4253=DIRECTION('',(0.,-1.,0.));
#4254=DIRECTION('',(0.,1.,0.));
#4255=DIRECTION('center_axis',(0.,-1.,0.));
#4256=DIRECTION('ref_axis',(0.,0.,-1.));
#4257=DIRECTION('',(0.,1.,0.));
#4258=DIRECTION('',(0.,-1.,0.));
#4259=DIRECTION('center_axis',(0.,1.,0.));
#4260=DIRECTION('ref_axis',(0.,0.,1.));
#4261=DIRECTION('center_axis',(0.,-1.,0.));
#4262=DIRECTION('ref_axis',(0.,0.,-1.));
#4263=DIRECTION('',(0.,-1.,0.));
#4264=DIRECTION('',(0.,1.,0.));
#4265=DIRECTION('center_axis',(0.,-1.,0.));
#4266=DIRECTION('ref_axis',(0.,0.,-1.));
#4267=DIRECTION('',(0.,1.,0.));
#4268=DIRECTION('',(0.,-1.,0.));
#4269=DIRECTION('center_axis',(0.,-1.,0.));
#4270=DIRECTION('ref_axis',(0.,0.,-1.));
#4271=DIRECTION('',(0.,-1.,0.));
#4272=DIRECTION('',(0.,1.,0.));
#4273=DIRECTION('center_axis',(0.,-1.,0.));
#4274=DIRECTION('ref_axis',(0.,0.,-1.));
#4275=DIRECTION('',(0.,1.,0.));
#4276=DIRECTION('',(0.,-1.,0.));
#4277=DIRECTION('center_axis',(0.,-1.,0.));
#4278=DIRECTION('ref_axis',(0.,0.,-1.));
#4279=DIRECTION('',(0.,-1.,0.));
#4280=DIRECTION('',(0.,1.,0.));
#4281=DIRECTION('center_axis',(0.,-1.,0.));
#4282=DIRECTION('ref_axis',(0.,0.,-1.));
#4283=DIRECTION('',(0.,1.,0.));
#4284=DIRECTION('',(0.,-1.,0.));
#4285=DIRECTION('center_axis',(-3.19907349870672E-11,5.57863918680909E-11,
-1.));
#4286=DIRECTION('ref_axis',(0.497276552988426,-0.86759208724374,-6.43080746094552E-11));
#4287=DIRECTION('center_axis',(1.44525360935827E-11,-2.51909259187994E-11,
-1.));
#4288=DIRECTION('ref_axis',(0.497276552986562,-0.867592087244808,2.90423553376484E-11));
#4289=DIRECTION('center_axis',(2.06438449760594E-11,-3.59885479736367E-11,
-1.));
#4290=DIRECTION('ref_axis',(0.497276552992529,-0.867592087241388,4.14890795036576E-11));
#4291=DIRECTION('center_axis',(2.49698601097415E-10,-4.35514137287291E-10,
-1.));
#4292=DIRECTION('ref_axis',(0.497276552985414,-0.867592087245466,5.02017879038053E-10));
#4293=DIRECTION('',(-0.000444989806894056,-0.497981067250872,-0.867187787416171));
#4294=DIRECTION('center_axis',(-1.08672663735946E-6,-0.999999999999405,
-9.69822234025278E-8));
#4295=DIRECTION('ref_axis',(-0.993173427402032,1.09062071306982E-6,-0.116647087838961));
#4296=DIRECTION('center_axis',(0.00428782528366409,0.999862759747476,-0.0160023818382871));
#4297=DIRECTION('ref_axis',(-0.996010901071261,0.0028439177098952,-0.0891863054469385));
#4298=DIRECTION('',(-0.866340788146811,0.499453339955959,0.));
#4299=DIRECTION('center_axis',(-1.,-3.60743552086608E-12,-2.06811073586693E-12));
#4300=DIRECTION('ref_axis',(4.15820547561974E-12,-0.867588616792801,-0.497282607791137));
#4301=DIRECTION('center_axis',(-1.,2.25457668866882E-10,1.29269218462105E-10));
#4302=DIRECTION('ref_axis',(-2.59887841129028E-10,-0.867588616793689,-0.497282607789588));
#4303=DIRECTION('center_axis',(-1.,2.36263581335445E-10,1.35502142240452E-10));
#4304=DIRECTION('ref_axis',(-2.72362452364694E-10,-0.867588616792773,-0.497282607791186));
#4305=DIRECTION('center_axis',(-1.,-8.29625555327683E-11,-4.75813038765708E-11));
#4306=DIRECTION('ref_axis',(9.56387236821049E-11,-0.867588616796214,-0.497282607785183));
#4307=DIRECTION('center_axis',(0.0317847666407182,0.865934893847345,-0.499145758498639));
#4308=DIRECTION('ref_axis',(-0.999494736640691,0.0275404977324392,-0.0158679681183856));
#4309=DIRECTION('center_axis',(7.10542735760101E-15,1.,-2.08198488598457E-15));
#4310=DIRECTION('ref_axis',(-1.,7.11179816109987E-15,-1.28035472349601E-15));
#4311=DIRECTION('',(7.105427357601E-15,-1.,-8.88178419700125E-16));
#4312=DIRECTION('',(-4.44089209850063E-16,1.,7.105427357601E-15));
#4313=DIRECTION('center_axis',(7.10542735760101E-15,1.,-2.08198488598457E-15));
#4314=DIRECTION('ref_axis',(-1.,7.11179816109987E-15,-1.28035472349601E-15));
#4315=DIRECTION('',(-7.105427357601E-15,1.,-8.88178419700125E-16));
#4316=DIRECTION('',(4.44089209850063E-16,-1.,1.4210854715202E-14));
#4317=DIRECTION('center_axis',(7.10542735760101E-15,1.,-2.08198488598457E-15));
#4318=DIRECTION('ref_axis',(-1.,7.11179816109987E-15,-1.28035472349601E-15));
#4319=DIRECTION('',(1.4210854715202E-14,-1.,0.));
#4320=DIRECTION('',(0.,1.,0.));
#4321=DIRECTION('center_axis',(7.10542735760101E-15,1.,-2.08198488598457E-15));
#4322=DIRECTION('ref_axis',(-1.,7.11179816109987E-15,-1.28035472349601E-15));
#4323=DIRECTION('',(-7.10542735760105E-15,1.,-8.88178419700132E-16));
#4324=DIRECTION('',(0.,-1.,7.105427357601E-15));
#4325=DIRECTION('center_axis',(7.10542735760101E-15,1.,-2.08198488598457E-15));
#4326=DIRECTION('ref_axis',(-1.,7.11179816109987E-15,-1.28035472349601E-15));
#4327=DIRECTION('',(1.4210854715202E-14,-1.,0.));
#4328=DIRECTION('',(-8.88178419700119E-16,1.,1.42108547152019E-14));
#4329=DIRECTION('center_axis',(7.10542735760101E-15,1.,-2.08198488598457E-15));
#4330=DIRECTION('ref_axis',(-1.,7.11179816109987E-15,-1.28035472349601E-15));
#4331=DIRECTION('',(-7.10542735760095E-15,1.,-8.88178419700119E-16));
#4332=DIRECTION('',(0.,-1.,7.10542735760095E-15));
#4333=DIRECTION('center_axis',(7.10542735760101E-15,1.,-2.08198488598457E-15));
#4334=DIRECTION('ref_axis',(-1.,7.11179816109987E-15,-1.28035472349601E-15));
#4335=DIRECTION('',(7.10542735760098E-15,-1.,-8.88178419700122E-16));
#4336=DIRECTION('',(-4.44089209850063E-16,1.,7.105427357601E-15));
#4337=DIRECTION('center_axis',(7.10542735760101E-15,1.,-2.08198488598457E-15));
#4338=DIRECTION('ref_axis',(-1.,7.11179816109987E-15,-1.28035472349601E-15));
#4339=DIRECTION('',(-7.10542735760095E-15,1.,0.));
#4340=DIRECTION('',(4.44089209850069E-16,-1.,7.1054273576011E-15));
#4341=DIRECTION('center_axis',(7.10542735760101E-15,1.,-2.08198488598457E-15));
#4342=DIRECTION('ref_axis',(-1.,7.11179816109987E-15,-1.28035472349601E-15));
#4343=DIRECTION('',(0.,1.,4.44089209850059E-16));
#4344=DIRECTION('',(-8.88178419700113E-16,-1.,-7.1054273576009E-15));
#4345=DIRECTION('center_axis',(7.10542735760101E-15,1.,-2.08198488598457E-15));
#4346=DIRECTION('ref_axis',(-1.,7.11179816109987E-15,-1.28035472349601E-15));
#4347=DIRECTION('',(7.105427357601E-15,1.,1.33226762955019E-15));
#4348=DIRECTION('',(-4.44089209850066E-16,-1.,-1.42108547152021E-14));
#4349=DIRECTION('center_axis',(7.10542735760101E-15,1.,-2.08198488598457E-15));
#4350=DIRECTION('ref_axis',(-1.,7.11179816109987E-15,-1.28035472349601E-15));
#4351=DIRECTION('',(-1.42108547152019E-14,-1.,4.44089209850059E-16));
#4352=DIRECTION('',(2.22044604925028E-15,1.,0.));
#4353=DIRECTION('center_axis',(7.10542735760101E-15,1.,-2.08198488598457E-15));
#4354=DIRECTION('ref_axis',(-1.,7.11179816109987E-15,-1.28035472349601E-15));
#4355=DIRECTION('',(7.105427357601E-15,1.,1.33226762955019E-15));
#4356=DIRECTION('',(0.,-1.,-1.42108547152018E-14));
#4357=DIRECTION('center_axis',(7.10542735760101E-15,1.,-2.08198488598457E-15));
#4358=DIRECTION('ref_axis',(-1.,7.11179816109987E-15,-1.28035472349601E-15));
#4359=DIRECTION('',(-7.10542735760095E-15,-1.,0.));
#4360=DIRECTION('',(0.,1.,-7.10542735760105E-15));
#4361=DIRECTION('center_axis',(7.10542735760101E-15,1.,-2.08198488598457E-15));
#4362=DIRECTION('ref_axis',(-1.,7.11179816109987E-15,-1.28035472349601E-15));
#4363=DIRECTION('',(7.105427357601E-15,1.,0.));
#4364=DIRECTION('',(-1.33226762955017E-15,-1.,0.));
#4365=DIRECTION('center_axis',(7.10542735760101E-15,1.,-2.08198488598457E-15));
#4366=DIRECTION('ref_axis',(-1.,7.11179816109987E-15,-1.28035472349601E-15));
#4367=DIRECTION('',(-7.105427357601E-15,-1.,0.));
#4368=DIRECTION('',(0.,1.,-7.1054273576011E-15));
#4369=DIRECTION('center_axis',(7.10542735760101E-15,1.,-2.08198488598457E-15));
#4370=DIRECTION('ref_axis',(-1.,7.11179816109987E-15,-1.28035472349601E-15));
#4371=DIRECTION('',(0.,1.,8.88178419700119E-16));
#4372=DIRECTION('',(0.,-0.999999999998377,1.80186440497577E-6));
#4373=DIRECTION('center_axis',(7.10542735760101E-15,1.,-2.08198488598457E-15));
#4374=DIRECTION('ref_axis',(-1.,7.11179816109987E-15,-1.28035472349601E-15));
#4375=DIRECTION('',(-7.10542735760095E-15,-1.,8.88178419700119E-16));
#4376=DIRECTION('',(-4.44089209850063E-16,1.,-7.105427357601E-15));
#4377=DIRECTION('center_axis',(7.10542735760101E-15,1.,-2.08198488598457E-15));
#4378=DIRECTION('ref_axis',(-1.,7.11179816109987E-15,-1.28035472349601E-15));
#4379=DIRECTION('',(0.,-1.,0.));
#4380=DIRECTION('',(0.,0.999999999996769,-2.54218367618327E-6));
#4381=DIRECTION('center_axis',(7.10542735760101E-15,1.,-2.08198488598457E-15));
#4382=DIRECTION('ref_axis',(-1.,7.11179816109987E-15,-1.28035472349601E-15));
#4383=DIRECTION('',(-7.10542735760098E-15,1.,0.));
#4384=DIRECTION('',(4.95945076311269E-14,0.498176579235464,0.867075599876534));
#4385=DIRECTION('center_axis',(-0.0160023818376506,-0.999862759747457,-0.00428782529044036));
#4386=DIRECTION('ref_axis',(0.320435510218814,-0.00106615058948748,-0.947269733029473));
#4387=DIRECTION('',(0.867428142068955,0.497562476827584,0.));
#4388=DIRECTION('',(-1.14214331302317E-14,-0.499456113421034,-0.866339189213068));
#4389=DIRECTION('center_axis',(2.06991832786293E-12,-3.59568180778876E-12,
-1.));
#4390=DIRECTION('ref_axis',(-0.497276552985882,0.867592087245198,-4.14890694656058E-12));
#4391=DIRECTION('center_axis',(-1.,-1.62328252343351E-10,-9.30760508218548E-11));
#4392=DIRECTION('ref_axis',(-1.87119245189999E-10,0.867588616794545,0.497282607788095));
#4393=DIRECTION('center_axis',(-2.05762092679575E-12,3.60273289486777E-12,
-1.));
#4394=DIRECTION('ref_axis',(-0.49727655299199,0.867592087241697,4.14890918496442E-12));
#4395=DIRECTION('center_axis',(-1.,-3.60038429955364E-12,-2.08040818675628E-12));
#4396=DIRECTION('ref_axis',(-4.15820323995394E-12,0.867588616794733,0.497282607787766));
#4397=DIRECTION('center_axis',(9.83463793864226E-13,-1.82736732563426E-12,
-1.));
#4398=DIRECTION('ref_axis',(-0.497276552989786,0.86759208724296,-2.07446291715088E-12));
#4399=DIRECTION('center_axis',(-1.,-7.20764353951641E-12,-4.14882635868306E-12));
#4400=DIRECTION('ref_axis',(-8.31640865557086E-12,0.867588616794545,0.497282607788095));
#4401=DIRECTION('center_axis',(-3.71471154516616E-10,6.47861553957569E-10,
-1.));
#4402=DIRECTION('ref_axis',(-0.497276552987665,0.867592087244176,7.46803453090951E-10));
#4403=DIRECTION('center_axis',(-1.,2.43483740809469E-10,1.39629140633371E-10));
#4404=DIRECTION('ref_axis',(2.80678865049538E-10,0.867588616792504,0.497282607791656));
#4405=DIRECTION('center_axis',(0.,1.,0.));
#4406=DIRECTION('ref_axis',(0.,0.,1.));
#4407=DIRECTION('',(0.,1.,0.));
#4408=DIRECTION('center_axis',(0.,1.,0.));
#4409=DIRECTION('ref_axis',(0.,0.,1.));
#4410=DIRECTION('',(0.,-1.,0.));
#4411=DIRECTION('center_axis',(0.,1.,0.));
#4412=DIRECTION('ref_axis',(0.,0.,1.));
#4413=DIRECTION('',(1.,0.,0.));
#4414=DIRECTION('center_axis',(0.,1.,0.));
#4415=DIRECTION('ref_axis',(0.,0.,1.));
#4416=DIRECTION('',(0.,0.,1.));
#4417=DIRECTION('center_axis',(0.,1.,0.));
#4418=DIRECTION('ref_axis',(0.,0.,1.));
#4419=DIRECTION('',(-1.,0.,0.));
#4420=DIRECTION('',(0.,0.,1.));
#4421=DIRECTION('center_axis',(0.,1.,0.));
#4422=DIRECTION('ref_axis',(0.,0.,1.));
#4423=DIRECTION('center_axis',(0.,1.,0.));
#4424=DIRECTION('ref_axis',(0.,0.,1.));
#4425=DIRECTION('',(1.,0.,0.));
#4426=DIRECTION('',(0.,0.,-1.));
#4427=DIRECTION('center_axis',(0.,1.,0.));
#4428=DIRECTION('ref_axis',(0.,0.,1.));
#4429=DIRECTION('',(-1.,0.,0.));
#4430=DIRECTION('',(0.,0.,-1.));
#4431=DIRECTION('center_axis',(0.,-1.,0.));
#4432=DIRECTION('ref_axis',(-7.6571373978539E-16,0.,1.));
#4433=DIRECTION('',(0.,-1.,0.));
#4434=DIRECTION('',(0.,1.,0.));
#4435=DIRECTION('center_axis',(0.,-1.,0.));
#4436=DIRECTION('ref_axis',(0.,0.,-1.));
#4437=DIRECTION('',(0.,1.,0.));
#4438=DIRECTION('center_axis',(0.,-1.,0.));
#4439=DIRECTION('ref_axis',(0.,0.,-1.));
#4440=DIRECTION('',(0.,-1.,0.));
#4441=DIRECTION('center_axis',(0.,-1.,0.));
#4442=DIRECTION('ref_axis',(0.,0.,-1.));
#4443=DIRECTION('',(0.,1.,0.));
#4444=DIRECTION('center_axis',(1.72297863328963E-10,-3.00549238109471E-10,
-1.));
#4445=DIRECTION('ref_axis',(0.497276552987805,-0.867592087244096,3.4643382838297E-10));
#4446=DIRECTION('',(-0.867432536984531,-0.497554814850163,2.89113612764477E-13));
#4447=DIRECTION('',(0.866169166920262,0.499750912231943,-1.16493376777939E-12));
#4448=DIRECTION('center_axis',(0.00452829227180621,-0.999846933665442,-0.0168998168307887));
#4449=DIRECTION('ref_axis',(0.987523822777422,0.0018110409973824,0.157459263232029));
#4450=DIRECTION('center_axis',(7.10542735760101E-15,1.,-2.08198488598457E-15));
#4451=DIRECTION('ref_axis',(-1.,7.11179816109987E-15,-1.28035472349601E-15));
#4452=DIRECTION('',(0.,-1.,-4.44089209850063E-16));
#4453=DIRECTION('center_axis',(7.10542735760101E-15,1.,-2.08198488598457E-15));
#4454=DIRECTION('ref_axis',(-1.,7.11179816109987E-15,-1.28035472349601E-15));
#4455=DIRECTION('',(0.,-1.,0.));
#4456=DIRECTION('',(7.105427357601E-15,1.,0.));
#4457=DIRECTION('center_axis',(7.10542735760101E-15,1.,-2.08198488598457E-15));
#4458=DIRECTION('ref_axis',(-1.,7.11179816109987E-15,-1.28035472349601E-15));
#4459=DIRECTION('',(-7.10542735760098E-15,1.,-4.44089209850061E-16));
#4460=DIRECTION('center_axis',(-1.29725002468514E-15,1.,1.01665643334203E-15));
#4461=DIRECTION('ref_axis',(-0.522944117603135,-1.55000729152176E-15,0.852366969012924));
#4462=DIRECTION('center_axis',(7.17477267547079E-12,-1.26249893789538E-11,
-1.));
#4463=DIRECTION('ref_axis',(-0.497276552987957,0.867592087244008,-1.45211870849278E-11));
#4464=DIRECTION('',(-0.866183392751839,-0.499726255184689,9.87106629258188E-14));
#4465=DIRECTION('center_axis',(-1.,0.,0.));
#4466=DIRECTION('ref_axis',(0.,0.,1.));
#4467=DIRECTION('',(-1.,0.,0.));
#4468=DIRECTION('',(-1.,0.,0.));
#4469=DIRECTION('',(1.,0.,0.));
#4470=DIRECTION('',(-1.,0.,0.));
#4471=DIRECTION('center_axis',(-1.,0.,0.));
#4472=DIRECTION('ref_axis',(0.,0.,1.));
#4473=DIRECTION('',(-1.,0.,0.));
#4474=DIRECTION('',(-1.,0.,0.));
#4475=DIRECTION('center_axis',(0.998237545662555,0.00530728060715426,0.0591069809934184));
#4476=DIRECTION('ref_axis',(0.0565541720181457,-0.386905875987754,-0.920383327072743));
#4477=DIRECTION('',(1.,0.,0.));
#4478=DIRECTION('',(-1.,0.,0.));
#4479=DIRECTION('center_axis',(0.,-1.,0.));
#4480=DIRECTION('ref_axis',(0.,0.,-1.));
#4481=DIRECTION('',(0.,1.,0.));
#4482=DIRECTION('center_axis',(0.,1.,0.));
#4483=DIRECTION('ref_axis',(0.,0.,1.));
#4484=DIRECTION('',(0.,1.,0.));
#4485=DIRECTION('center_axis',(0.,0.,-1.));
#4486=DIRECTION('ref_axis',(-1.,0.,0.));
#4487=DIRECTION('',(0.,0.,-1.));
#4488=DIRECTION('',(0.,0.,-1.));
#4489=DIRECTION('center_axis',(0.,-1.,0.));
#4490=DIRECTION('ref_axis',(0.,0.,-1.));
#4491=DIRECTION('center_axis',(0.,-1.,0.));
#4492=DIRECTION('ref_axis',(0.,0.,-1.));
#4493=DIRECTION('center_axis',(0.,-1.,0.));
#4494=DIRECTION('ref_axis',(0.,0.,-1.));
#4495=DIRECTION('center_axis',(0.,-1.,0.));
#4496=DIRECTION('ref_axis',(0.,0.,-1.));
#4497=DIRECTION('center_axis',(0.,1.,0.));
#4498=DIRECTION('ref_axis',(0.,0.,1.));
#4499=DIRECTION('center_axis',(0.,-1.,0.));
#4500=DIRECTION('ref_axis',(0.,0.,-1.));
#4501=DIRECTION('center_axis',(0.,0.,-1.));
#4502=DIRECTION('ref_axis',(-1.,0.,0.));
#4503=DIRECTION('',(0.,0.,-1.));
#4504=DIRECTION('',(0.,0.,-1.));
#4505=DIRECTION('center_axis',(1.,1.27629810543002E-16,0.));
#4506=DIRECTION('ref_axis',(-1.27629810543002E-16,1.,0.));
#4507=DIRECTION('center_axis',(-1.,0.,0.));
#4508=DIRECTION('ref_axis',(0.,0.,1.));
#4509=DIRECTION('center_axis',(1.,1.27629810543002E-16,0.));
#4510=DIRECTION('ref_axis',(-1.27629810543002E-16,1.,0.));
#4511=DIRECTION('center_axis',(-1.,0.,0.));
#4512=DIRECTION('ref_axis',(0.,0.,1.));
#4513=DIRECTION('center_axis',(0.,0.,-1.));
#4514=DIRECTION('ref_axis',(-1.,0.,0.));
#4515=DIRECTION('center_axis',(0.,-1.40464835892948E-16,1.));
#4516=DIRECTION('ref_axis',(0.,-1.,-1.40464835892948E-16));
#4517=DIRECTION('center_axis',(0.,0.,-1.));
#4518=DIRECTION('ref_axis',(-1.,0.,0.));
#4519=DIRECTION('center_axis',(0.,-1.40464835892948E-16,1.));
#4520=DIRECTION('ref_axis',(0.,-1.,-1.40464835892948E-16));
#4521=DIRECTION('center_axis',(0.,-1.40464835892948E-16,1.));
#4522=DIRECTION('ref_axis',(0.,-1.,-1.40464835892948E-16));
#4523=DIRECTION('center_axis',(0.,-1.,0.));
#4524=DIRECTION('ref_axis',(0.,0.,-1.));
#4525=DIRECTION('axis',(0.,0.,1.));
#4526=DIRECTION('refdir',(1.,0.,0.));
#4527=DIRECTION('center_axis',(-1.14604935876865E-29,1.,6.74466494129217E-15));
#4528=DIRECTION('ref_axis',(1.,0.,1.79134021914735E-15));
#4529=DIRECTION('',(-1.14604935876865E-29,1.,6.74466494129217E-15));
#4530=DIRECTION('center_axis',(0.,-1.,0.));
#4531=DIRECTION('ref_axis',(1.,0.,1.79134021914735E-15));
#4532=DIRECTION('',(-3.46872215696891E-7,0.999999999999934,1.12705778808245E-7));
#4533=DIRECTION('center_axis',(-1.14604935876865E-29,1.,6.74466494129217E-15));
#4534=DIRECTION('ref_axis',(1.,0.,1.79134021914735E-15));
#4535=DIRECTION('',(-1.14604935876865E-29,1.,6.74466494129217E-15));
#4536=DIRECTION('center_axis',(-1.14604935876865E-29,1.,6.74466494129217E-15));
#4537=DIRECTION('ref_axis',(1.,0.,1.79134021914735E-15));
#4538=DIRECTION('',(-1.14604935876865E-29,1.,6.74466494129217E-15));
#4539=DIRECTION('center_axis',(-1.14604935876865E-29,1.,6.74466494129217E-15));
#4540=DIRECTION('ref_axis',(1.,0.,1.79134021914735E-15));
#4541=DIRECTION('',(-1.14604935876865E-29,1.,6.74466494129217E-15));
#4542=DIRECTION('',(0.,-1.,-3.46944695195361E-16));
#4543=DIRECTION('center_axis',(0.,-1.,0.));
#4544=DIRECTION('ref_axis',(0.,0.,-1.));
#4545=DIRECTION('',(0.,-1.,0.));
#4546=DIRECTION('center_axis',(0.,1.,0.));
#4547=DIRECTION('ref_axis',(0.,0.,1.));
#4548=DIRECTION('center_axis',(0.,-1.,0.));
#4549=DIRECTION('ref_axis',(0.,0.,-1.));
#4550=DIRECTION('',(0.,-1.,0.));
#4551=DIRECTION('',(0.,1.,0.));
#4552=DIRECTION('center_axis',(0.,1.,0.));
#4553=DIRECTION('ref_axis',(0.,0.,1.));
#4554=DIRECTION('center_axis',(0.,-1.,0.));
#4555=DIRECTION('ref_axis',(0.,0.,-1.));
#4556=DIRECTION('',(0.,-1.,0.));
#4557=DIRECTION('center_axis',(0.,-1.,0.));
#4558=DIRECTION('ref_axis',(0.,0.,-1.));
#4559=DIRECTION('',(0.,-1.,0.));
#4560=DIRECTION('',(3.46872213130258E-7,-0.999999999999933,-1.1270548577469E-7));
#4561=DIRECTION('center_axis',(0.,1.,0.));
#4562=DIRECTION('ref_axis',(0.,0.,1.));
#4563=DIRECTION('center_axis',(0.,1.,0.));
#4564=DIRECTION('ref_axis',(0.,0.,1.));
#4565=DIRECTION('center_axis',(0.,1.,0.));
#4566=DIRECTION('ref_axis',(0.,0.,1.));
#4567=DIRECTION('',(0.,1.,0.));
#4568=DIRECTION('center_axis',(0.,1.,0.));
#4569=DIRECTION('ref_axis',(0.,0.,1.));
#4570=DIRECTION('center_axis',(0.,1.,0.));
#4571=DIRECTION('ref_axis',(0.,0.,1.));
#4572=DIRECTION('center_axis',(0.,1.,0.));
#4573=DIRECTION('ref_axis',(0.,0.,1.));
#4574=DIRECTION('',(0.,1.,0.));
#4575=DIRECTION('center_axis',(0.,1.,0.));
#4576=DIRECTION('ref_axis',(0.,0.,1.));
#4577=DIRECTION('center_axis',(0.,-1.,0.));
#4578=DIRECTION('ref_axis',(0.,0.,-1.));
#4579=DIRECTION('center_axis',(0.,1.,0.));
#4580=DIRECTION('ref_axis',(0.,0.,1.));
#4581=DIRECTION('',(0.,1.,0.));
#4582=DIRECTION('center_axis',(0.,1.,0.));
#4583=DIRECTION('ref_axis',(0.,0.,1.));
#4584=DIRECTION('center_axis',(0.,-1.,0.));
#4585=DIRECTION('ref_axis',(0.,0.,-1.));
#4586=DIRECTION('center_axis',(0.,1.,0.));
#4587=DIRECTION('ref_axis',(0.,0.,1.));
#4588=DIRECTION('',(0.,-1.,0.));
#4589=DIRECTION('center_axis',(0.,1.,0.));
#4590=DIRECTION('ref_axis',(0.,0.,1.));
#4591=DIRECTION('center_axis',(0.,-1.,0.));
#4592=DIRECTION('ref_axis',(0.,0.,-1.));
#4593=DIRECTION('center_axis',(-0.951056619716827,-3.64722989082937E-7,
0.30901667607537));
#4594=DIRECTION('ref_axis',(0.309016676075391,1.57739547043686E-23,0.95105661971689));
#4595=DIRECTION('',(-0.309016676075391,0.,-0.95105661971689));
#4596=DIRECTION('',(-0.267616460838902,0.500000023942052,-0.82363912361301));
#4597=DIRECTION('center_axis',(-1.14604935876865E-29,1.,6.74466494129217E-15));
#4598=DIRECTION('ref_axis',(1.,0.,1.79134021914735E-15));
#4599=DIRECTION('',(-0.866025403784441,-0.499999999999996,0.));
#4600=DIRECTION('center_axis',(0.,1.,0.));
#4601=DIRECTION('ref_axis',(0.,0.,1.));
#4602=DIRECTION('center_axis',(0.,1.,0.));
#4603=DIRECTION('ref_axis',(0.,0.,1.));
#4604=DIRECTION('center_axis',(0.,0.,1.));
#4605=DIRECTION('ref_axis',(1.,0.,0.));
#4606=DIRECTION('',(0.866025403784441,-0.499999999999996,1.38777878684589E-16));
#4607=DIRECTION('center_axis',(0.,1.,0.));
#4608=DIRECTION('ref_axis',(0.,0.,1.));
#4609=DIRECTION('center_axis',(0.,1.,0.));
#4610=DIRECTION('ref_axis',(0.,0.,1.));
#4611=DIRECTION('center_axis',(0.,1.,0.));
#4612=DIRECTION('ref_axis',(0.,0.,1.));
#4613=DIRECTION('axis',(0.,0.,1.));
#4614=DIRECTION('refdir',(1.,0.,0.));
#4615=DIRECTION('center_axis',(4.93038065763132E-32,2.46519032881566E-32,
-1.));
#4616=DIRECTION('ref_axis',(-1.,-5.55111512312578E-17,-4.93038065763132E-32));
#4617=DIRECTION('center_axis',(-4.93038065763132E-32,-2.46519032881566E-32,
1.));
#4618=DIRECTION('ref_axis',(1.,5.55111512312578E-17,4.93038065763132E-32));
#4619=DIRECTION('',(-4.93038065763132E-32,-2.46519032881566E-32,1.));
#4620=DIRECTION('center_axis',(-4.93038065763132E-32,-2.46519032881566E-32,
1.));
#4621=DIRECTION('ref_axis',(1.,5.55111512312578E-17,4.93038065763132E-32));
#4622=DIRECTION('center_axis',(4.93038065763132E-32,-2.46519032881566E-32,
1.));
#4623=DIRECTION('ref_axis',(1.,5.55111512312578E-17,-4.93038065763132E-32));
#4624=DIRECTION('center_axis',(4.93038065763132E-32,-2.46519032881566E-32,
1.));
#4625=DIRECTION('ref_axis',(1.,5.55111512312578E-17,-4.93038065763132E-32));
#4626=DIRECTION('axis',(0.,0.,1.));
#4627=DIRECTION('refdir',(1.,0.,0.));
#4628=DIRECTION('center_axis',(0.,0.,-1.));
#4629=DIRECTION('ref_axis',(-1.,0.,0.));
#4630=DIRECTION('center_axis',(0.,0.,1.));
#4631=DIRECTION('ref_axis',(1.,0.,0.));
#4632=DIRECTION('',(0.,0.,-1.));
#4633=DIRECTION('center_axis',(0.,0.,1.));
#4634=DIRECTION('ref_axis',(1.,0.,0.));
#4635=DIRECTION('center_axis',(0.,0.,-1.));
#4636=DIRECTION('ref_axis',(-1.,0.,0.));
#4637=DIRECTION('center_axis',(0.,0.,1.));
#4638=DIRECTION('ref_axis',(1.,0.,0.));
#4639=DIRECTION('',(0.,0.,1.));
#4640=DIRECTION('center_axis',(0.,0.,1.));
#4641=DIRECTION('ref_axis',(1.,0.,0.));
#4642=DIRECTION('center_axis',(0.,0.,1.));
#4643=DIRECTION('ref_axis',(1.,0.,0.));
#4644=DIRECTION('center_axis',(0.,0.,1.));
#4645=DIRECTION('ref_axis',(1.,0.,0.));
#4646=DIRECTION('axis',(0.,0.,1.));
#4647=DIRECTION('refdir',(1.,0.,0.));
#4648=DIRECTION('center_axis',(0.,-1.,0.));
#4649=DIRECTION('ref_axis',(0.,0.,-1.));
#4650=DIRECTION('center_axis',(0.,1.,0.));
#4651=DIRECTION('ref_axis',(0.,0.,1.));
#4652=DIRECTION('',(0.,-1.,0.));
#4653=DIRECTION('center_axis',(0.,1.,0.));
#4654=DIRECTION('ref_axis',(0.,0.,1.));
#4655=DIRECTION('center_axis',(0.,-1.,0.));
#4656=DIRECTION('ref_axis',(0.,0.,-1.));
#4657=DIRECTION('center_axis',(0.,1.,0.));
#4658=DIRECTION('ref_axis',(0.,0.,1.));
#4659=DIRECTION('',(0.,1.,0.));
#4660=DIRECTION('center_axis',(0.,1.,0.));
#4661=DIRECTION('ref_axis',(0.,0.,1.));
#4662=DIRECTION('center_axis',(0.,1.,0.));
#4663=DIRECTION('ref_axis',(0.,0.,1.));
#4664=DIRECTION('center_axis',(0.,1.,0.));
#4665=DIRECTION('ref_axis',(0.,0.,1.));
#4666=DIRECTION('axis',(0.,0.,1.));
#4667=DIRECTION('refdir',(1.,0.,0.));
#4668=DIRECTION('center_axis',(0.,1.,0.));
#4669=DIRECTION('ref_axis',(0.,0.,1.));
#4670=DIRECTION('center_axis',(0.,1.,0.));
#4671=DIRECTION('ref_axis',(0.,0.,1.));
#4672=DIRECTION('',(0.,1.,0.));
#4673=DIRECTION('center_axis',(0.,1.,0.));
#4674=DIRECTION('ref_axis',(0.,0.,1.));
#4675=DIRECTION('center_axis',(0.,1.,0.));
#4676=DIRECTION('ref_axis',(0.,0.,1.));
#4677=DIRECTION('center_axis',(0.,1.,0.));
#4678=DIRECTION('ref_axis',(0.,0.,1.));
#4679=DIRECTION('',(0.,1.,0.));
#4680=DIRECTION('center_axis',(0.,1.,0.));
#4681=DIRECTION('ref_axis',(0.,0.,1.));
#4682=DIRECTION('center_axis',(0.,-1.,0.));
#4683=DIRECTION('ref_axis',(0.,0.,-1.));
#4684=DIRECTION('center_axis',(0.,1.,0.));
#4685=DIRECTION('ref_axis',(0.,0.,1.));
#4686=DIRECTION('',(0.,-1.,0.));
#4687=DIRECTION('center_axis',(0.,1.,0.));
#4688=DIRECTION('ref_axis',(0.,0.,1.));
#4689=DIRECTION('center_axis',(0.,-1.,0.));
#4690=DIRECTION('ref_axis',(0.,0.,-1.));
#4691=DIRECTION('center_axis',(0.,1.,0.));
#4692=DIRECTION('ref_axis',(0.,0.,1.));
#4693=DIRECTION('',(0.,-1.,0.));
#4694=DIRECTION('center_axis',(0.,1.,0.));
#4695=DIRECTION('ref_axis',(0.,0.,1.));
#4696=DIRECTION('center_axis',(0.,-1.,0.));
#4697=DIRECTION('ref_axis',(0.,0.,-1.));
#4698=DIRECTION('center_axis',(0.,1.,0.));
#4699=DIRECTION('ref_axis',(0.,0.,1.));
#4700=DIRECTION('',(0.,-1.,0.));
#4701=DIRECTION('center_axis',(0.,1.,0.));
#4702=DIRECTION('ref_axis',(0.,0.,1.));
#4703=DIRECTION('center_axis',(0.,-1.,0.));
#4704=DIRECTION('ref_axis',(0.,0.,-1.));
#4705=DIRECTION('center_axis',(0.,1.,0.));
#4706=DIRECTION('ref_axis',(0.,0.,1.));
#4707=DIRECTION('',(0.,-1.,0.));
#4708=DIRECTION('center_axis',(0.,1.,0.));
#4709=DIRECTION('ref_axis',(0.,0.,1.));
#4710=DIRECTION('center_axis',(0.,-1.,0.));
#4711=DIRECTION('ref_axis',(0.,0.,-1.));
#4712=DIRECTION('center_axis',(0.,1.,0.));
#4713=DIRECTION('ref_axis',(0.,0.,1.));
#4714=DIRECTION('',(0.,1.,0.));
#4715=DIRECTION('center_axis',(0.,1.,0.));
#4716=DIRECTION('ref_axis',(0.,0.,1.));
#4717=DIRECTION('center_axis',(0.,1.,0.));
#4718=DIRECTION('ref_axis',(0.,0.,1.));
#4719=DIRECTION('center_axis',(0.,1.,0.));
#4720=DIRECTION('ref_axis',(0.,0.,1.));
#4721=DIRECTION('center_axis',(0.,1.,0.));
#4722=DIRECTION('ref_axis',(0.,0.,1.));
#4723=DIRECTION('axis',(0.,0.,1.));
#4724=DIRECTION('refdir',(1.,0.,0.));
#4725=DIRECTION('center_axis',(-1.,0.,0.));
#4726=DIRECTION('ref_axis',(0.,0.,1.));
#4727=DIRECTION('',(0.,-1.,0.));
#4728=DIRECTION('',(0.,0.,-1.));
#4729=DIRECTION('',(0.,1.,0.));
#4730=DIRECTION('',(0.,0.,1.));
#4731=DIRECTION('center_axis',(0.,0.,1.));
#4732=DIRECTION('ref_axis',(1.,0.,0.));
#4733=DIRECTION('',(0.,-1.,0.));
#4734=DIRECTION('',(-1.,0.,0.));
#4735=DIRECTION('',(0.,1.,0.));
#4736=DIRECTION('',(1.,0.,0.));
#4737=DIRECTION('center_axis',(1.,0.,0.));
#4738=DIRECTION('ref_axis',(0.,0.,-1.));
#4739=DIRECTION('',(0.,-1.,0.));
#4740=DIRECTION('',(0.,0.,1.));
#4741=DIRECTION('',(0.,1.,0.));
#4742=DIRECTION('',(0.,0.,-1.));
#4743=DIRECTION('center_axis',(0.,0.,-1.));
#4744=DIRECTION('ref_axis',(-1.,0.,0.));
#4745=DIRECTION('',(0.,-1.,0.));
#4746=DIRECTION('',(1.,0.,0.));
#4747=DIRECTION('',(0.,1.,0.));
#4748=DIRECTION('',(-1.,0.,0.));
#4749=DIRECTION('center_axis',(0.,-1.,0.));
#4750=DIRECTION('ref_axis',(0.,0.,-1.));
#4751=DIRECTION('',(0.,0.,1.));
#4752=DIRECTION('',(1.,0.,0.));
#4753=DIRECTION('',(0.,0.,-1.));
#4754=DIRECTION('',(-1.,0.,0.));
#4755=DIRECTION('center_axis',(0.,-1.,0.));
#4756=DIRECTION('ref_axis',(0.,0.,-1.));
#4757=DIRECTION('',(0.,0.,-1.));
#4758=DIRECTION('',(1.,0.,0.));
#4759=DIRECTION('',(0.,0.,1.));
#4760=DIRECTION('',(-1.,0.,0.));
#4761=DIRECTION('center_axis',(0.,-1.,0.));
#4762=DIRECTION('ref_axis',(0.,0.,-1.));
#4763=DIRECTION('center_axis',(0.,1.,0.));
#4764=DIRECTION('ref_axis',(0.,0.,1.));
#4765=DIRECTION('center_axis',(0.,-1.,0.));
#4766=DIRECTION('ref_axis',(0.,0.,-1.));
#4767=DIRECTION('center_axis',(0.,1.,0.));
#4768=DIRECTION('ref_axis',(0.,0.,1.));
#4769=DIRECTION('center_axis',(1.,0.,0.));
#4770=DIRECTION('ref_axis',(0.,0.,1.));
#4771=DIRECTION('center_axis',(0.,-8.67361737988404E-16,1.));
#4772=DIRECTION('ref_axis',(0.,1.,8.67361737988404E-16));
#4773=DIRECTION('center_axis',(1.,0.,0.));
#4774=DIRECTION('ref_axis',(0.,1.,-8.88178419700125E-16));
#4775=DIRECTION('center_axis',(-8.67361737988403E-16,0.,1.));
#4776=DIRECTION('ref_axis',(-1.,0.,-8.67361737988403E-16));
#4777=DIRECTION('center_axis',(1.,0.,0.));
#4778=DIRECTION('ref_axis',(0.,0.,1.));
#4779=DIRECTION('center_axis',(0.,0.,1.));
#4780=DIRECTION('ref_axis',(1.,0.,0.));
#4781=DIRECTION('center_axis',(0.,0.,1.));
#4782=DIRECTION('ref_axis',(1.,0.,0.));
#4783=DIRECTION('center_axis',(-1.,0.,0.));
#4784=DIRECTION('ref_axis',(0.,0.,1.));
#4785=DIRECTION('center_axis',(1.,0.,0.));
#4786=DIRECTION('ref_axis',(0.,0.,-1.));
#4787=DIRECTION('center_axis',(0.,-1.,0.));
#4788=DIRECTION('ref_axis',(0.,0.,-1.));
#4789=DIRECTION('center_axis',(0.,-1.,0.));
#4790=DIRECTION('ref_axis',(0.,0.,-1.));
#4791=DIRECTION('center_axis',(0.,1.,0.));
#4792=DIRECTION('ref_axis',(0.,0.,1.));
#4793=DIRECTION('center_axis',(1.,0.,0.));
#4794=DIRECTION('ref_axis',(0.,0.,-1.));
#4795=DIRECTION('center_axis',(1.,0.,0.));
#4796=DIRECTION('ref_axis',(0.,0.,-1.));
#4797=DIRECTION('center_axis',(0.,0.,-1.));
#4798=DIRECTION('ref_axis',(-1.,0.,0.));
#4799=DIRECTION('center_axis',(0.,0.,1.));
#4800=DIRECTION('ref_axis',(1.,0.,0.));
#4801=DIRECTION('center_axis',(0.,-1.,0.));
#4802=DIRECTION('ref_axis',(0.,0.,-1.));
#4803=DIRECTION('center_axis',(0.,1.,0.));
#4804=DIRECTION('ref_axis',(0.,0.,1.));
#4805=DIRECTION('center_axis',(0.,-1.,0.));
#4806=DIRECTION('ref_axis',(0.,0.,-1.));
#4807=DIRECTION('center_axis',(0.,1.,0.));
#4808=DIRECTION('ref_axis',(0.,0.,1.));
#4809=DIRECTION('center_axis',(1.,0.,0.));
#4810=DIRECTION('ref_axis',(0.,0.,1.));
#4811=DIRECTION('center_axis',(0.,1.,0.));
#4812=DIRECTION('ref_axis',(-1.,0.,0.));
#4813=DIRECTION('center_axis',(0.,0.,1.));
#4814=DIRECTION('ref_axis',(-1.,0.,0.));
#4815=DIRECTION('center_axis',(1.,0.,0.));
#4816=DIRECTION('ref_axis',(0.,1.,-8.88178419700125E-16));
#4817=DIRECTION('center_axis',(0.,0.,1.));
#4818=DIRECTION('ref_axis',(-1.,0.,0.));
#4819=DIRECTION('center_axis',(0.,0.,1.));
#4820=DIRECTION('ref_axis',(0.,-1.,0.));
#4821=DIRECTION('center_axis',(1.,0.,0.));
#4822=DIRECTION('ref_axis',(0.,0.,1.));
#4823=DIRECTION('center_axis',(1.,0.,0.));
#4824=DIRECTION('ref_axis',(0.,0.,-1.));
#4825=DIRECTION('center_axis',(1.,0.,0.));
#4826=DIRECTION('ref_axis',(0.,0.,-1.));
#4827=DIRECTION('center_axis',(0.,0.,-1.));
#4828=DIRECTION('ref_axis',(-1.,0.,0.));
#4829=DIRECTION('center_axis',(0.,0.,1.));
#4830=DIRECTION('ref_axis',(1.,0.,0.));
#4831=DIRECTION('center_axis',(0.,0.,1.));
#4832=DIRECTION('ref_axis',(1.,0.,0.));
#4833=DIRECTION('center_axis',(0.,0.,1.));
#4834=DIRECTION('ref_axis',(1.,0.,0.));
#4835=DIRECTION('center_axis',(-1.,0.,0.));
#4836=DIRECTION('ref_axis',(0.,0.,1.));
#4837=DIRECTION('center_axis',(1.,0.,0.));
#4838=DIRECTION('ref_axis',(0.,0.,-1.));
#4839=DIRECTION('center_axis',(1.,0.,0.));
#4840=DIRECTION('ref_axis',(0.,0.,1.));
#4841=DIRECTION('center_axis',(0.,-1.,0.));
#4842=DIRECTION('ref_axis',(0.,0.,1.));
#4843=DIRECTION('center_axis',(1.,0.,0.));
#4844=DIRECTION('ref_axis',(0.,0.,-1.));
#4845=DIRECTION('center_axis',(0.,1.,0.));
#4846=DIRECTION('ref_axis',(0.,0.,-1.));
#4847=DIRECTION('center_axis',(0.,-1.,0.));
#4848=DIRECTION('ref_axis',(0.,0.,-1.));
#4849=DIRECTION('axis',(0.,0.,1.));
#4850=DIRECTION('refdir',(1.,0.,0.));
#4851=DIRECTION('center_axis',(1.11022302462516E-16,-1.,0.));
#4852=DIRECTION('ref_axis',(0.,0.,-1.));
#4853=DIRECTION('center_axis',(-1.11022302462516E-16,1.,0.));
#4854=DIRECTION('ref_axis',(0.,0.,1.));
#4855=DIRECTION('',(-1.11022302462516E-16,1.,0.));
#4856=DIRECTION('center_axis',(-1.11022302462516E-16,1.,0.));
#4857=DIRECTION('ref_axis',(0.,0.,1.));
#4858=DIRECTION('center_axis',(-1.11022302462516E-16,1.,0.));
#4859=DIRECTION('ref_axis',(0.,0.,1.));
#4860=DIRECTION('center_axis',(-1.11022302462516E-16,1.,0.));
#4861=DIRECTION('ref_axis',(0.,0.,1.));
#4862=DIRECTION('axis',(0.,0.,1.));
#4863=DIRECTION('refdir',(1.,0.,0.));
#4864=DIRECTION('center_axis',(0.,1.,0.));
#4865=DIRECTION('ref_axis',(0.,0.,1.));
#4866=DIRECTION('center_axis',(0.,1.,0.));
#4867=DIRECTION('ref_axis',(0.,0.,1.));
#4868=DIRECTION('center_axis',(0.,-1.,0.));
#4869=DIRECTION('ref_axis',(0.,0.,1.));
#4870=DIRECTION('center_axis',(0.,1.,0.));
#4871=DIRECTION('ref_axis',(0.,0.,1.));
#4872=DIRECTION('center_axis',(0.,1.,0.));
#4873=DIRECTION('ref_axis',(0.,0.,1.));
#4874=DIRECTION('',(0.,1.,0.));
#4875=DIRECTION('center_axis',(0.,-1.,0.));
#4876=DIRECTION('ref_axis',(0.,0.,-1.));
#4877=DIRECTION('',(0.,-1.,0.));
#4878=DIRECTION('center_axis',(-0.888342258257525,-0.459181916231379,-4.393783563666E-14));
#4879=DIRECTION('ref_axis',(0.459181916231379,-0.888342258257525,-4.20136709809981E-13));
#4880=DIRECTION('center_axis',(0.906925322797953,-0.42129141798502,3.93873602430886E-13));
#4881=DIRECTION('ref_axis',(0.42129141798502,0.906925322797953,-2.61951590649629E-13));
#4882=DIRECTION('',(0.,1.,0.));
#4883=DIRECTION('center_axis',(0.,-1.,0.));
#4884=DIRECTION('ref_axis',(0.,0.,-1.));
#4885=DIRECTION('center_axis',(0.,-1.,0.));
#4886=DIRECTION('ref_axis',(0.,0.,-1.));
#4887=DIRECTION('center_axis',(0.,1.,0.));
#4888=DIRECTION('ref_axis',(0.,0.,1.));
#4889=DIRECTION('center_axis',(0.,1.,0.));
#4890=DIRECTION('ref_axis',(0.,0.,1.));
#4891=DIRECTION('',(0.,1.,0.));
#4892=DIRECTION('center_axis',(0.,1.,0.));
#4893=DIRECTION('ref_axis',(0.,0.,1.));
#4894=DIRECTION('center_axis',(-0.888342258257544,-0.459181916231341,-3.75501605328633E-13));
#4895=DIRECTION('ref_axis',(0.459181916231341,-0.888342258257545,-8.50644926987111E-13));
#4896=DIRECTION('',(0.,-1.,0.));
#4897=DIRECTION('center_axis',(0.,-1.,0.));
#4898=DIRECTION('ref_axis',(0.,0.,-1.));
#4899=DIRECTION('',(0.,1.,0.));
#4900=DIRECTION('center_axis',(0.906925322797957,-0.421291417985012,2.87289631591583E-13));
#4901=DIRECTION('ref_axis',(0.421291417985012,0.906925322797957,-1.29853851007989E-12));
#4902=DIRECTION('center_axis',(0.,1.,0.));
#4903=DIRECTION('ref_axis',(0.,0.,1.));
#4904=DIRECTION('center_axis',(0.,1.,0.));
#4905=DIRECTION('ref_axis',(0.,0.,1.));
#4906=DIRECTION('center_axis',(0.,1.,0.));
#4907=DIRECTION('ref_axis',(0.,0.,1.));
#4908=DIRECTION('center_axis',(0.,1.,0.));
#4909=DIRECTION('ref_axis',(0.,0.,1.));
#4910=DIRECTION('center_axis',(0.,1.,0.));
#4911=DIRECTION('ref_axis',(0.,0.,1.));
#4912=DIRECTION('center_axis',(0.,-1.,0.));
#4913=DIRECTION('ref_axis',(0.,0.,-1.));
#4914=DIRECTION('center_axis',(0.,1.,0.));
#4915=DIRECTION('ref_axis',(0.,0.,1.));
#4916=DIRECTION('',(0.,0.,-1.));
#4917=DIRECTION('',(0.,0.,1.));
#4918=DIRECTION('center_axis',(1.,0.,0.));
#4919=DIRECTION('ref_axis',(0.,0.,-1.));
#4920=DIRECTION('',(0.,0.,1.));
#4921=DIRECTION('',(0.,0.,1.));
#4922=DIRECTION('center_axis',(0.,-1.,0.));
#4923=DIRECTION('ref_axis',(0.,0.,-1.));
#4924=DIRECTION('',(0.,0.,1.));
#4925=DIRECTION('center_axis',(-1.,-1.16210731118036E-16,-1.36736175538941E-63));
#4926=DIRECTION('ref_axis',(1.16210731118036E-16,-1.,-6.16297582203915E-33));
#4927=DIRECTION('',(0.,0.,1.));
#4928=DIRECTION('center_axis',(-0.888342258257513,-0.459181916231401,1.66533453693773E-16));
#4929=DIRECTION('ref_axis',(0.459181916231401,-0.888342258257513,-9.95253396589023E-33));
#4930=DIRECTION('center_axis',(0.906925322797977,-0.421291417984968,5.55111512312578E-17));
#4931=DIRECTION('ref_axis',(0.421291417984968,0.906925322797977,2.77555756156289E-17));
#4932=DIRECTION('center_axis',(0.,1.,0.));
#4933=DIRECTION('ref_axis',(1.,0.,1.03372647248395E-14));
#4934=DIRECTION('center_axis',(0.,1.,0.));
#4935=DIRECTION('ref_axis',(0.,0.,1.));
#4936=DIRECTION('',(0.,0.,1.));
#4937=DIRECTION('',(1.,0.,0.));
#4938=DIRECTION('',(-1.,0.,1.04744440165294E-14));
#4939=DIRECTION('',(1.04744440165294E-14,0.,1.));
#4940=DIRECTION('',(0.,0.,1.));
#4941=DIRECTION('',(0.961261695938319,0.275637355817,0.));
#4942=DIRECTION('',(0.,0.,1.));
#4943=DIRECTION('',(1.,0.,0.));
#4944=DIRECTION('',(0.,0.,1.));
#4945=DIRECTION('',(1.,0.,0.));
#4946=DIRECTION('',(0.,0.,1.));
#4947=DIRECTION('',(1.,0.,0.));
#4948=DIRECTION('',(0.0191477946218101,0.,0.999816664174548));
#4949=DIRECTION('',(0.999816664174548,0.,-0.0191477946218101));
#4950=DIRECTION('',(6.17858228010388E-17,1.,-2.02148675015649E-16));
#4951=DIRECTION('',(0.645379358927795,-1.94289029309402E-16,-0.763862214715421));
#4952=DIRECTION('',(0.,-1.,0.));
#4953=DIRECTION('',(1.,0.,0.));
#4954=DIRECTION('',(0.,0.,1.));
#4955=DIRECTION('',(1.,0.,0.));
#4956=DIRECTION('',(-0.0244891147268135,0.,0.999700096658942));
#4957=DIRECTION('',(0.999700096658942,0.,0.0244891147268135));
#4958=DIRECTION('',(0.,0.,1.));
#4959=DIRECTION('',(1.,0.,0.));
#4960=DIRECTION('',(-1.,4.05398043168549E-32,-3.49148133884313E-15));
#4961=DIRECTION('',(-3.35622727311334E-15,0.275637355817,0.961261695938319));
#4962=DIRECTION('',(6.98296267768627E-15,-2.83602643198701E-32,-1.));
#4963=DIRECTION('',(-0.961261695938319,0.275637355817,-6.71245454622668E-15));
#4964=DIRECTION('',(1.,3.18834639255818E-31,1.04744440165294E-14));
#4965=DIRECTION('',(1.006868181934E-14,0.275637355817,-0.961261695938319));
#4966=DIRECTION('',(-0.866025403784443,0.,-0.499999999999992));
#4967=DIRECTION('',(-0.499999999999992,0.,0.866025403784443));
#4968=DIRECTION('',(-0.500000000000007,0.,-0.866025403784435));
#4969=DIRECTION('',(-0.866025403784435,0.,0.500000000000007));
#4970=DIRECTION('',(-6.98296267768627E-15,0.,-1.));
#4971=DIRECTION('',(-1.,0.,6.98296267768627E-15));
#4972=DIRECTION('',(0.499999999999995,0.,-0.866025403784442));
#4973=DIRECTION('',(-0.866025403784442,0.,-0.499999999999995));
#4974=DIRECTION('',(0.866025403784436,0.,-0.500000000000004));
#4975=DIRECTION('',(-0.500000000000004,0.,-0.866025403784436));
#4976=DIRECTION('',(1.,0.,-3.49148133884313E-15));
#4977=DIRECTION('',(-3.49148133884313E-15,0.,-1.));
#4978=DIRECTION('',(0.86602540378444,0.,0.499999999999998));
#4979=DIRECTION('',(0.499999999999998,0.,-0.86602540378444));
#4980=DIRECTION('',(0.500000000000001,0.,0.866025403784438));
#4981=DIRECTION('',(0.866025403784438,0.,-0.500000000000001));
#4982=DIRECTION('',(0.,0.,1.));
#4983=DIRECTION('',(1.,0.,0.));
#4984=DIRECTION('',(-0.500000000000001,0.,0.866025403784438));
#4985=DIRECTION('',(0.866025403784438,0.,0.500000000000001));
#4986=DIRECTION('',(-0.86602540378444,0.,0.499999999999998));
#4987=DIRECTION('',(0.499999999999998,0.,0.86602540378444));
#4988=CARTESIAN_POINT('',(0.,0.,0.));
#4989=CARTESIAN_POINT('',(0.,0.,0.));
#4990=CARTESIAN_POINT('Origin',(150.,0.,0.));
#4991=CARTESIAN_POINT('',(150.,4.86031698411606E-16,-146.03125));
#4992=CARTESIAN_POINT('Origin',(150.,0.,-150.));
#4993=CARTESIAN_POINT('Origin',(150.,-4.86031698411606E-16,0.));
#4994=CARTESIAN_POINT('',(0.,0.,0.));
#4995=CARTESIAN_POINT('Origin',(216.,0.,0.));
#4996=CARTESIAN_POINT('',(0.,-4.86031698411606E-16,-3.96875));
#4997=CARTESIAN_POINT('Origin',(0.,0.,0.));
#4998=CARTESIAN_POINT('',(216.,-4.86031698411606E-16,-3.96875));
#4999=CARTESIAN_POINT('',(216.,-4.86031698411606E-16,-3.96875));
#5000=CARTESIAN_POINT('Origin',(216.,0.,0.));
#5001=CARTESIAN_POINT('Origin',(216.,0.,0.));
#5002=CARTESIAN_POINT('Origin',(0.,0.,0.));
#5003=CARTESIAN_POINT('',(0.,0.,0.));
#5004=CARTESIAN_POINT('Origin',(0.,0.,220.));
#5005=CARTESIAN_POINT('',(3.96875,-4.86031698411606E-16,0.));
#5006=CARTESIAN_POINT('Origin',(0.,0.,0.));
#5007=CARTESIAN_POINT('',(3.96875,-4.86031698411606E-16,220.));
#5008=CARTESIAN_POINT('',(3.96875,-4.86031698411606E-16,220.));
#5009=CARTESIAN_POINT('Origin',(0.,0.,220.));
#5010=CARTESIAN_POINT('Origin',(0.,0.,220.));
#5011=CARTESIAN_POINT('Origin',(0.,0.,0.));
#5012=CARTESIAN_POINT('',(0.,0.,0.));
#5013=CARTESIAN_POINT('Origin',(0.,3.42,0.));
#5014=CARTESIAN_POINT('',(-4.89858719658941E-15,3.42,40.));
#5015=CARTESIAN_POINT('Origin',(0.,3.42,0.));
#5016=CARTESIAN_POINT('',(-4.89858719658941E-15,0.,40.));
#5017=CARTESIAN_POINT('',(-4.89858719658941E-15,3.42,40.));
#5018=CARTESIAN_POINT('Origin',(0.,0.,0.));
#5019=CARTESIAN_POINT('Origin',(0.,60.,0.));
#5020=CARTESIAN_POINT('',(-5.63337527607782E-15,0.,46.));
#5021=CARTESIAN_POINT('Origin',(0.,0.,0.));
#5022=CARTESIAN_POINT('',(-5.63337527607782E-15,20.,46.));
#5023=CARTESIAN_POINT('',(-5.63337527607782E-15,60.,46.));
#5024=CARTESIAN_POINT('Origin',(0.,20.,0.));
#5025=CARTESIAN_POINT('Origin',(0.,20.,0.));
#5026=CARTESIAN_POINT('',(39.8660227411065,28.,3.27112072623103));
#5027=CARTESIAN_POINT('',(-39.8660227411065,28.,3.27112072623103));
#5028=CARTESIAN_POINT('Origin',(0.,28.,0.));
#5029=CARTESIAN_POINT('',(-39.8000405653402,28.,-3.99459271982449));
#5030=CARTESIAN_POINT('Ctrl Pts',(-39.8000405653402,28.,-3.99459271982449));
#5031=CARTESIAN_POINT('Ctrl Pts',(-39.8202648350751,27.541880505153,-3.79308863359818));
#5032=CARTESIAN_POINT('Ctrl Pts',(-39.8478595264142,27.1249694755492,-3.5013875154554));
#5033=CARTESIAN_POINT('Ctrl Pts',(-39.902305612745,26.4396195203269,-2.81616960677907));
#5034=CARTESIAN_POINT('Ctrl Pts',(-39.9327182501717,26.1341927725789,-2.37013786718776));
#5035=CARTESIAN_POINT('Ctrl Pts',(-39.9787551488202,25.728954292425,-1.39236385403762));
#5036=CARTESIAN_POINT('Ctrl Pts',(-39.9938528018644,25.629163825102,-0.860588043983172));
#5037=CARTESIAN_POINT('Ctrl Pts',(-40.0028726554704,25.629163825102,0.136767468615171));
#5038=CARTESIAN_POINT('Ctrl Pts',(-39.9974053268697,25.7288296122476,0.668382268299115));
#5039=CARTESIAN_POINT('Ctrl Pts',(-39.9691084018832,26.1338587427398,1.64606843741232));
#5040=CARTESIAN_POINT('Ctrl Pts',(-39.9468068466375,26.4392073572614,2.09216112009085));
#5041=CARTESIAN_POINT('Ctrl Pts',(-39.90483592212,27.124631969712,2.77769565092216));
#5042=CARTESIAN_POINT('Ctrl Pts',(-39.8825619687711,27.5417352224658,3.06955273734297));
#5043=CARTESIAN_POINT('Ctrl Pts',(-39.8660227411065,28.,3.27112072623103));
#5044=CARTESIAN_POINT('',(-4.89858719658941E-15,28.,-40.));
#5045=CARTESIAN_POINT('Origin',(0.,28.,0.));
#5046=CARTESIAN_POINT('',(-4.89858719658941E-15,20.,-40.));
#5047=CARTESIAN_POINT('',(-4.89858719658941E-15,20.,-40.));
#5048=CARTESIAN_POINT('Origin',(0.,20.,0.));
#5049=CARTESIAN_POINT('',(39.8000405653402,28.,-3.99459271982449));
#5050=CARTESIAN_POINT('Origin',(0.,28.,0.));
#5051=CARTESIAN_POINT('Ctrl Pts',(39.8660227411065,28.,3.27112072623103));
#5052=CARTESIAN_POINT('Ctrl Pts',(39.8825619687711,27.5417352224658,3.06955273734297));
#5053=CARTESIAN_POINT('Ctrl Pts',(39.90483592212,27.124631969712,2.77769565092216));
#5054=CARTESIAN_POINT('Ctrl Pts',(39.9468068466375,26.4392073572614,2.09216112009085));
#5055=CARTESIAN_POINT('Ctrl Pts',(39.9691084018832,26.1338587427398,1.64606843741232));
#5056=CARTESIAN_POINT('Ctrl Pts',(39.9974053268697,25.7288296122476,0.668382268299116));
#5057=CARTESIAN_POINT('Ctrl Pts',(40.0028726554704,25.629163825102,0.136767468615172));
#5058=CARTESIAN_POINT('Ctrl Pts',(39.9938528018644,25.629163825102,-0.860588043983171));
#5059=CARTESIAN_POINT('Ctrl Pts',(39.9787551488202,25.728954292425,-1.39236385403762));
#5060=CARTESIAN_POINT('Ctrl Pts',(39.9327182501717,26.1341927725789,-2.37013786718776));
#5061=CARTESIAN_POINT('Ctrl Pts',(39.902305612745,26.4396195203269,-2.81616960677907));
#5062=CARTESIAN_POINT('Ctrl Pts',(39.8478595264142,27.1249694755492,-3.5013875154554));
#5063=CARTESIAN_POINT('Ctrl Pts',(39.8202648350751,27.541880505153,-3.79308863359818));
#5064=CARTESIAN_POINT('Ctrl Pts',(39.8000405653402,28.,-3.99459271982449));
#5065=CARTESIAN_POINT('Origin',(0.,60.,0.));
#5066=CARTESIAN_POINT('',(-45.7957082162897,30.5508791552084,-4.33048599679682));
#5067=CARTESIAN_POINT('',(45.8192253759653,28.1946814357457,-4.07413622090531));
#5068=CARTESIAN_POINT('Ctrl Pts',(-45.7957082162897,30.5508791552084,-4.3304859967968));
#5069=CARTESIAN_POINT('Ctrl Pts',(-45.2904567403498,30.4582791384642,-9.67361588686245));
#5070=CARTESIAN_POINT('Ctrl Pts',(-43.8539847608527,30.3636491983601,-14.8873227195869));
#5071=CARTESIAN_POINT('Ctrl Pts',(-39.2595475939355,30.1793388276773,-24.5606349388711));
#5072=CARTESIAN_POINT('Ctrl Pts',(-36.1445477184839,30.089019872629,-28.9501043330206));
#5073=CARTESIAN_POINT('Ctrl Pts',(-28.0998693561851,29.8910356446895,-36.9061963106983));
#5074=CARTESIAN_POINT('Ctrl Pts',(-23.0758554236481,29.7911290471386,-40.2389742761901));
#5075=CARTESIAN_POINT('Ctrl Pts',(-11.9484440491057,29.5822410004833,-44.83339037117));
#5076=CARTESIAN_POINT('Ctrl Pts',(-5.93853076275596,29.4754507871743,-46.0166322639478));
#5077=CARTESIAN_POINT('Ctrl Pts',(6.19463923460001,29.2702187768307,-45.9830112670864));
#5078=CARTESIAN_POINT('Ctrl Pts',(12.1989476144052,29.1632197696209,-44.7660144128937));
#5079=CARTESIAN_POINT('Ctrl Pts',(23.3037531300962,28.9544249372012,-40.1078138073594));
#5080=CARTESIAN_POINT('Ctrl Pts',(28.3109481824939,28.8543575036543,-36.744954507633));
#5081=CARTESIAN_POINT('Ctrl Pts',(36.3100560865774,28.6563561267642,-28.7419061208428));
#5082=CARTESIAN_POINT('Ctrl Pts',(39.398809462358,28.5662371851081,-24.3362112688292));
#5083=CARTESIAN_POINT('Ctrl Pts',(43.9371605347039,28.3817876471969,-14.6396372497778));
#5084=CARTESIAN_POINT('Ctrl Pts',(45.3439760357657,28.2871742724011,-9.4189640439544));
#5085=CARTESIAN_POINT('Ctrl Pts',(45.8192253759654,28.1946814357456,-4.07413622090525));
#5086=CARTESIAN_POINT('',(45.8262286142197,28.,-3.99459271982449));
#5087=CARTESIAN_POINT('Origin',(46.0952922108427,29.6008626071972,-0.378516324486955));
#5088=CARTESIAN_POINT('',(-45.8262286142197,28.,-3.99459271982449));
#5089=CARTESIAN_POINT('Origin',(0.,28.,0.));
#5090=CARTESIAN_POINT('',(-45.7957082162897,29.597913825102,-4.33048599679673));
#5091=CARTESIAN_POINT('Ctrl Pts',(-45.7957082162897,29.597913825102,-4.33048599679673));
#5092=CARTESIAN_POINT('Ctrl Pts',(-45.7957082162897,29.0993094464563,-4.33048599679673));
#5093=CARTESIAN_POINT('Ctrl Pts',(-45.8054776929032,28.5676691611987,-4.23078571512148));
#5094=CARTESIAN_POINT('Ctrl Pts',(-45.8242431489185,28.0524370568086,-4.01732005107389));
#5095=CARTESIAN_POINT('Ctrl Pts',(-45.8252258288706,28.0261543846796,-4.00609673885219));
#5096=CARTESIAN_POINT('Ctrl Pts',(-45.8262286142197,28.,-3.99459271982449));
#5097=CARTESIAN_POINT('',(-45.7957082162897,60.,-4.33048599679673));
#5098=CARTESIAN_POINT('Origin',(0.,60.,0.));
#5099=CARTESIAN_POINT('',(3.61293045337858,36.9438035983105,-35.8182458188427));
#5100=CARTESIAN_POINT('',(-4.32456637758084,36.9438035983105,-35.7393078506831));
#5101=CARTESIAN_POINT('Ctrl Pts',(-4.32456637758084,36.9438035983105,-35.7393078506831));
#5102=CARTESIAN_POINT('Ctrl Pts',(-4.32456637758084,36.4450208015675,-35.7393078506831));
#5103=CARTESIAN_POINT('Ctrl Pts',(-4.22479607288452,35.9133171831831,-35.7518200690335));
#5104=CARTESIAN_POINT('Ctrl Pts',(-3.81972115078383,34.9357522694673,-35.7973640118356));
#5105=CARTESIAN_POINT('Ctrl Pts',(-3.51444243124228,34.4898519148477,-35.8297856438023));
#5106=CARTESIAN_POINT('Ctrl Pts',(-2.81035536837098,33.7856002162544,-35.891877281823));
#5107=CARTESIAN_POINT('Ctrl Pts',(-2.36438104223203,33.4801763497608,-35.9256086610747));
#5108=CARTESIAN_POINT('Ctrl Pts',(-1.38661844382939,33.074889941751,-35.9766166372815));
#5109=CARTESIAN_POINT('Ctrl Pts',(-0.854788951444588,32.9750535983105,-35.9933095700074));
#5110=CARTESIAN_POINT('Ctrl Pts',(0.142732488159273,32.9750535983105,-36.0031693423161));
#5111=CARTESIAN_POINT('Ctrl Pts',(0.67436622526082,33.0747383580536,-35.9970058845568));
#5112=CARTESIAN_POINT('Ctrl Pts',(1.65202206260133,33.4797702852856,-35.9654003949313));
#5113=CARTESIAN_POINT('Ctrl Pts',(2.09807056759484,33.7850992008905,-35.9405439624699));
#5114=CARTESIAN_POINT('Ctrl Pts',(2.80252582511813,34.489417022928,-35.8924857314627));
#5115=CARTESIAN_POINT('Ctrl Pts',(3.10796993106093,34.9355112883736,-35.8661668197574));
#5116=CARTESIAN_POINT('Ctrl Pts',(3.51318310448797,35.913320036691,-35.828744662717));
#5117=CARTESIAN_POINT('Ctrl Pts',(3.61293362241916,36.44506523213,-35.8182454991865));
#5118=CARTESIAN_POINT('Ctrl Pts',(3.61293362241916,36.9438035983105,-35.8182454991865));
#5119=CARTESIAN_POINT('',(-4.32456003949879,57.,-35.73930861761));
#5120=CARTESIAN_POINT('',(-4.32456003949879,60.,-35.73930861761));
#5121=CARTESIAN_POINT('',(-35.7385910610862,57.,-4.33048599679673));
#5122=CARTESIAN_POINT('Origin',(0.,57.,0.));
#5123=CARTESIAN_POINT('',(-35.7385910610862,29.597913825102,-4.33048599679673));
#5124=CARTESIAN_POINT('',(-35.7385910610862,60.,-4.33048599679673));
#5125=CARTESIAN_POINT('',(-35.8188421083191,29.597913825102,3.60701400320327));
#5126=CARTESIAN_POINT('Ctrl Pts',(-35.7385910610862,29.597913825102,-4.33048599679673));
#5127=CARTESIAN_POINT('Ctrl Pts',(-35.7385910610862,29.0991306962933,-4.33048599679673));
#5128=CARTESIAN_POINT('Ctrl Pts',(-35.7511200860441,28.5674275274957,-4.23071553786938));
#5129=CARTESIAN_POINT('Ctrl Pts',(-35.7967317559948,27.5898649766328,-3.8256420007237));
#5130=CARTESIAN_POINT('Ctrl Pts',(-35.8292042530398,27.1439664630341,-3.52036488637474));
#5131=CARTESIAN_POINT('Ctrl Pts',(-35.8914128483252,26.4397150924934,-2.81628112104011));
#5132=CARTESIAN_POINT('Ctrl Pts',(-35.925218216728,26.1342902091051,-2.37030719253055));
#5133=CARTESIAN_POINT('Ctrl Pts',(-35.9763878543241,25.7290014455195,-1.39254337628737));
#5134=CARTESIAN_POINT('Ctrl Pts',(-35.9931684759662,25.629163825102,-0.860712147213517));
#5135=CARTESIAN_POINT('Ctrl Pts',(-36.0031923000525,25.629163825102,0.13680939481454));
#5136=CARTESIAN_POINT('Ctrl Pts',(-35.9971163491985,25.7288473393432,0.66844161100349));
#5137=CARTESIAN_POINT('Ctrl Pts',(-35.9656720315245,26.1338773873715,1.64609688970905));
#5138=CARTESIAN_POINT('Ctrl Pts',(-35.9408892795961,26.4392057398786,2.09214623166637));
#5139=CARTESIAN_POINT('Ctrl Pts',(-35.8929475807102,27.1435243342817,2.79660431841842));
#5140=CARTESIAN_POINT('Ctrl Pts',(-35.8666793391538,27.5896199855471,3.10204957133501));
#5141=CARTESIAN_POINT('Ctrl Pts',(-35.8293245843937,28.5674304286977,3.50726366036052));
#5142=CARTESIAN_POINT('Ctrl Pts',(-35.8188421083191,29.0991758664567,3.60701400320327));
#5143=CARTESIAN_POINT('Ctrl Pts',(-35.8188421083191,29.597913825102,3.60701400320327));
#5144=CARTESIAN_POINT('',(-35.8188421083191,57.,3.60701400320327));
#5145=CARTESIAN_POINT('',(-35.8188421083191,60.,3.60701400320327));
#5146=CARTESIAN_POINT('',(-4.32456003949879,57.,35.73930861761));
#5147=CARTESIAN_POINT('Origin',(0.,57.,0.));
#5148=CARTESIAN_POINT('',(-4.32456320853981,36.9438035983105,35.7393079465999));
#5149=CARTESIAN_POINT('',(-4.32456003949879,57.,35.73930861761));
#5150=CARTESIAN_POINT('',(2.49793749409559E-11,32.9910360529178,36.));
#5151=CARTESIAN_POINT('Ctrl Pts',(-4.32456637758084,36.9438035983105,35.7393078506831));
#5152=CARTESIAN_POINT('Ctrl Pts',(-4.32456637758084,36.4450208015675,35.7393078506831));
#5153=CARTESIAN_POINT('Ctrl Pts',(-4.22479607288452,35.9133171831831,35.7518200690335));
#5154=CARTESIAN_POINT('Ctrl Pts',(-3.81972115078383,34.9357522694673,35.7973640118356));
#5155=CARTESIAN_POINT('Ctrl Pts',(-3.51444243124228,34.4898519148477,35.8297856438023));
#5156=CARTESIAN_POINT('Ctrl Pts',(-2.81035536837098,33.7856002162544,35.891877281823));
#5157=CARTESIAN_POINT('Ctrl Pts',(-2.36438104223203,33.4801763497608,35.9256086610747));
#5158=CARTESIAN_POINT('Ctrl Pts',(-1.38661844382939,33.074889941751,35.9766166372815));
#5159=CARTESIAN_POINT('Ctrl Pts',(-0.854788951444588,32.9750535983105,35.9933095700074));
#5160=CARTESIAN_POINT('Ctrl Pts',(-0.238725233717463,32.9750535983105,35.9993989107907));
#5161=CARTESIAN_POINT('Ctrl Pts',(-0.119781262522339,32.9802536999292,36.));
#5162=CARTESIAN_POINT('Ctrl Pts',(4.99631239159193E-11,32.9910360529178,
36.));
#5163=CARTESIAN_POINT('',(-4.40872847693047E-15,3.42,36.));
#5164=CARTESIAN_POINT('',(-4.40872847693047E-15,60.,36.));
#5165=CARTESIAN_POINT('Origin',(0.,3.42,0.));
#5166=CARTESIAN_POINT('',(3.61293362241916,36.9438035983105,35.8182454991865));
#5167=CARTESIAN_POINT('Ctrl Pts',(4.99630892214498E-11,32.9910360529178,
36.));
#5168=CARTESIAN_POINT('Ctrl Pts',(0.390221549150756,33.0261626361231,36.));
#5169=CARTESIAN_POINT('Ctrl Pts',(0.78917426933185,33.1223020523269,35.99329438987));
#5170=CARTESIAN_POINT('Ctrl Pts',(1.65202206260133,33.4797702852856,35.9654003949313));
#5171=CARTESIAN_POINT('Ctrl Pts',(2.09807056759484,33.7850992008905,35.9405439624699));
#5172=CARTESIAN_POINT('Ctrl Pts',(2.80252582511813,34.489417022928,35.8924857314627));
#5173=CARTESIAN_POINT('Ctrl Pts',(3.10796993106093,34.9355112883736,35.8661668197574));
#5174=CARTESIAN_POINT('Ctrl Pts',(3.51318310448797,35.913320036691,35.828744662717));
#5175=CARTESIAN_POINT('Ctrl Pts',(3.61293362241916,36.44506523213,35.8182454991865));
#5176=CARTESIAN_POINT('Ctrl Pts',(3.61293362241916,36.9438035983105,35.8182454991865));
#5177=CARTESIAN_POINT('',(3.61292728433799,57.,35.8182461384988));
#5178=CARTESIAN_POINT('',(3.61292728433799,60.,35.8182461384988));
#5179=CARTESIAN_POINT('',(35.8188421083191,57.,3.60701400320327));
#5180=CARTESIAN_POINT('Origin',(0.,57.,0.));
#5181=CARTESIAN_POINT('',(35.8188421083191,29.597913825102,3.60701400320327));
#5182=CARTESIAN_POINT('',(35.8188421083191,60.,3.60701400320327));
#5183=CARTESIAN_POINT('',(35.7385910610862,29.597913825102,-4.33048599679673));
#5184=CARTESIAN_POINT('Ctrl Pts',(35.8188421083191,29.597913825102,3.60701400320327));
#5185=CARTESIAN_POINT('Ctrl Pts',(35.8188421083191,29.0991758664567,3.60701400320327));
#5186=CARTESIAN_POINT('Ctrl Pts',(35.8293245843937,28.5674304286977,3.50726366036052));
#5187=CARTESIAN_POINT('Ctrl Pts',(35.8666793391538,27.589619985547,3.102049571335));
#5188=CARTESIAN_POINT('Ctrl Pts',(35.8929475807102,27.1435243342817,2.79660431841842));
#5189=CARTESIAN_POINT('Ctrl Pts',(35.9408892795961,26.4392057398786,2.09214623166637));
#5190=CARTESIAN_POINT('Ctrl Pts',(35.9656720315245,26.1338773873715,1.64609688970904));
#5191=CARTESIAN_POINT('Ctrl Pts',(35.9971163491985,25.7288473393432,0.668441611003487));
#5192=CARTESIAN_POINT('Ctrl Pts',(36.0031923000525,25.629163825102,0.13680939481454));
#5193=CARTESIAN_POINT('Ctrl Pts',(35.9931684759662,25.629163825102,-0.860712147213517));
#5194=CARTESIAN_POINT('Ctrl Pts',(35.9763878543241,25.7290014455195,-1.39254337628737));
#5195=CARTESIAN_POINT('Ctrl Pts',(35.925218216728,26.1342902091051,-2.37030719253055));
#5196=CARTESIAN_POINT('Ctrl Pts',(35.8914128483252,26.4397150924934,-2.81628112104011));
#5197=CARTESIAN_POINT('Ctrl Pts',(35.8292042530398,27.1439664630341,-3.52036488637474));
#5198=CARTESIAN_POINT('Ctrl Pts',(35.7967317559948,27.5898649766328,-3.8256420007237));
#5199=CARTESIAN_POINT('Ctrl Pts',(35.7511200860441,28.5674275274957,-4.23071553786938));
#5200=CARTESIAN_POINT('Ctrl Pts',(35.7385910610862,29.0991306962933,-4.33048599679673));
#5201=CARTESIAN_POINT('Ctrl Pts',(35.7385910610862,29.597913825102,-4.33048599679673));
#5202=CARTESIAN_POINT('',(35.7385910610862,57.,-4.33048599679673));
#5203=CARTESIAN_POINT('',(35.7385910610862,60.,-4.33048599679673));
#5204=CARTESIAN_POINT('',(3.61292728433799,57.,-35.8182461384988));
#5205=CARTESIAN_POINT('Origin',(0.,57.,0.));
#5206=CARTESIAN_POINT('',(3.61292728433799,60.,-35.8182461384988));
#5207=CARTESIAN_POINT('Origin',(0.,60.,0.));
#5208=CARTESIAN_POINT('',(45.7957082162897,37.5741208584476,-4.33048599679664));
#5209=CARTESIAN_POINT('',(45.7957082162897,38.1991208721035,-4.33048599679673));
#5210=CARTESIAN_POINT('',(45.7957082162897,60.,-4.33048599679673));
#5211=CARTESIAN_POINT('',(3.61292728433797,38.688289262853,-45.8578974271399));
#5212=CARTESIAN_POINT('Ctrl Pts',(3.61292728433797,38.688289262853,-45.8578974271399));
#5213=CARTESIAN_POINT('Ctrl Pts',(13.9875081498765,38.5092320746522,-45.0405331698223));
#5214=CARTESIAN_POINT('Ctrl Pts',(23.,38.3333333333333,-39.8371685740842));
#5215=CARTESIAN_POINT('Ctrl Pts',(33.6743371481683,38.125,-33.6743371481684));
#5216=CARTESIAN_POINT('Ctrl Pts',(39.8371685740842,37.9166666666667,-23.));
#5217=CARTESIAN_POINT('Ctrl Pts',(44.8515840435634,37.7471553142903,-14.3147776366026));
#5218=CARTESIAN_POINT('Ctrl Pts',(45.7957082162897,37.5741208584476,-4.33048599679664));
#5219=CARTESIAN_POINT('',(3.61292728433799,39.3132892765089,-45.8578974271399));
#5220=CARTESIAN_POINT('',(3.61292728433799,60.,-45.8578974271399));
#5221=CARTESIAN_POINT('Ctrl Pts',(3.61292728433799,39.3132892765089,-45.8578974271399));
#5222=CARTESIAN_POINT('Ctrl Pts',(13.9875081498766,39.1342320883081,-45.0405331698222));
#5223=CARTESIAN_POINT('Ctrl Pts',(23.,38.9583333469893,-39.8371685740842));
#5224=CARTESIAN_POINT('Ctrl Pts',(33.6743371481683,38.7500000136559,-33.6743371481684));
#5225=CARTESIAN_POINT('Ctrl Pts',(39.8371685740842,38.5416666803226,-23.));
#5226=CARTESIAN_POINT('Ctrl Pts',(44.8515840435634,38.3721553279462,-14.3147776366027));
#5227=CARTESIAN_POINT('Ctrl Pts',(45.7957082162897,38.1991208721035,-4.33048599679673));
#5228=CARTESIAN_POINT('Origin',(0.,60.,0.));
#5229=CARTESIAN_POINT('',(45.858362923034,38.0633913333999,3.60701400320327));
#5230=CARTESIAN_POINT('',(45.858362923034,37.438391319744,3.60701400320326));
#5231=CARTESIAN_POINT('',(45.858362923034,60.,3.60701400320327));
#5232=CARTESIAN_POINT('',(3.61292728433719,36.9367107508029,45.85789742714));
#5233=CARTESIAN_POINT('Ctrl Pts',(45.858362923034,38.0633913333999,3.60701400320327));
#5234=CARTESIAN_POINT('Ctrl Pts',(45.0420919829705,37.8842847836873,13.9848082063042));
#5235=CARTESIAN_POINT('Ctrl Pts',(39.8371685740842,37.7083333469893,23.));
#5236=CARTESIAN_POINT('Ctrl Pts',(33.6743371481684,37.5000000136559,33.6743371481683));
#5237=CARTESIAN_POINT('Ctrl Pts',(23.,37.2916666803226,39.8371685740842));
#5238=CARTESIAN_POINT('Ctrl Pts',(13.9875081498762,37.1157679390038,45.0405331698225));
#5239=CARTESIAN_POINT('Ctrl Pts',(3.61292728433719,36.9367107508029,45.85789742714));
#5240=CARTESIAN_POINT('',(3.56213286848811,36.3108341932617,45.8618709760868));
#5241=CARTESIAN_POINT('Ctrl Pts',(3.56213286848809,36.3108341932617,45.8618709760868));
#5242=CARTESIAN_POINT('Ctrl Pts',(3.59615968466946,36.5214531232455,45.8592280825949));
#5243=CARTESIAN_POINT('Ctrl Pts',(3.61256125750481,36.7319034897672,45.8579262646664));
#5244=CARTESIAN_POINT('Ctrl Pts',(3.61292728433716,36.9367107508029,45.85789742714));
#5245=CARTESIAN_POINT('Ctrl Pts',(45.858362923034,37.438391319744,3.60701400320326));
#5246=CARTESIAN_POINT('Ctrl Pts',(45.0420919829705,37.2592847700314,13.9848082063042));
#5247=CARTESIAN_POINT('Ctrl Pts',(39.8371685740842,37.0833333333333,23.));
#5248=CARTESIAN_POINT('Ctrl Pts',(33.6743371481684,36.875,33.6743371481683));
#5249=CARTESIAN_POINT('Ctrl Pts',(23.,36.6666666666667,39.8371685740842));
#5250=CARTESIAN_POINT('Ctrl Pts',(13.9643142594927,36.490315245202,45.0539241686789));
#5251=CARTESIAN_POINT('Ctrl Pts',(3.56213286848811,36.3108341932617,45.8618709760868));
#5252=CARTESIAN_POINT('Origin',(0.,60.,0.));
#5253=CARTESIAN_POINT('',(45.7957082162897,52.5741208584476,-4.33048599679672));
#5254=CARTESIAN_POINT('',(45.7957082162897,53.1991208721035,-4.33048599679673));
#5255=CARTESIAN_POINT('',(45.7957082162897,60.,-4.33048599679673));
#5256=CARTESIAN_POINT('',(3.61292728433801,53.688289262853,-45.8578974271399));
#5257=CARTESIAN_POINT('Ctrl Pts',(3.61292728433801,53.688289262853,-45.8578974271399));
#5258=CARTESIAN_POINT('Ctrl Pts',(13.9875081498766,53.5092320746522,-45.0405331698222));
#5259=CARTESIAN_POINT('Ctrl Pts',(23.,53.3333333333333,-39.8371685740842));
#5260=CARTESIAN_POINT('Ctrl Pts',(33.6743371481683,53.125,-33.6743371481684));
#5261=CARTESIAN_POINT('Ctrl Pts',(39.8371685740842,52.9166666666667,-23.));
#5262=CARTESIAN_POINT('Ctrl Pts',(44.8515840435634,52.7471553142902,-14.3147776366027));
#5263=CARTESIAN_POINT('Ctrl Pts',(45.7957082162897,52.5741208584476,-4.33048599679672));
#5264=CARTESIAN_POINT('',(3.61292728433799,54.3132892765089,-45.8578974271399));
#5265=CARTESIAN_POINT('',(3.61292728433799,60.,-45.8578974271399));
#5266=CARTESIAN_POINT('Ctrl Pts',(3.61292728433799,54.3132892765089,-45.8578974271399));
#5267=CARTESIAN_POINT('Ctrl Pts',(13.9875081498766,54.1342320883081,-45.0405331698223));
#5268=CARTESIAN_POINT('Ctrl Pts',(23.,53.9583333469893,-39.8371685740842));
#5269=CARTESIAN_POINT('Ctrl Pts',(33.6743371481683,53.7500000136559,-33.6743371481684));
#5270=CARTESIAN_POINT('Ctrl Pts',(39.8371685740842,53.5416666803226,-23.));
#5271=CARTESIAN_POINT('Ctrl Pts',(44.8515840435634,53.3721553279462,-14.3147776366027));
#5272=CARTESIAN_POINT('Ctrl Pts',(45.7957082162897,53.1991208721035,-4.33048599679673));
#5273=CARTESIAN_POINT('Origin',(0.,60.,0.));
#5274=CARTESIAN_POINT('',(45.858362923034,53.0633913333999,3.60701400320327));
#5275=CARTESIAN_POINT('',(45.858362923034,52.438391319744,3.60701400320324));
#5276=CARTESIAN_POINT('',(45.858362923034,60.,3.60701400320327));
#5277=CARTESIAN_POINT('',(3.612927284338,51.936710750803,45.8578974271399));
#5278=CARTESIAN_POINT('Ctrl Pts',(45.858362923034,53.0633913333999,3.60701400320327));
#5279=CARTESIAN_POINT('Ctrl Pts',(45.0420919829705,52.8842847836873,13.9848082063043));
#5280=CARTESIAN_POINT('Ctrl Pts',(39.8371685740842,52.7083333469893,23.));
#5281=CARTESIAN_POINT('Ctrl Pts',(33.6743371481684,52.5000000136559,33.6743371481683));
#5282=CARTESIAN_POINT('Ctrl Pts',(23.,52.2916666803226,39.8371685740842));
#5283=CARTESIAN_POINT('Ctrl Pts',(13.9875081498766,52.1157679390038,45.0405331698223));
#5284=CARTESIAN_POINT('Ctrl Pts',(3.612927284338,51.9367107508029,45.8578974271399));
#5285=CARTESIAN_POINT('',(3.61292728433799,51.311710737147,45.8578974271399));
#5286=CARTESIAN_POINT('',(3.61292728433799,60.,45.8578974271399));
#5287=CARTESIAN_POINT('Ctrl Pts',(45.858362923034,52.438391319744,3.60701400320324));
#5288=CARTESIAN_POINT('Ctrl Pts',(45.0420919829705,52.2592847700314,13.9848082063043));
#5289=CARTESIAN_POINT('Ctrl Pts',(39.8371685740842,52.0833333333333,23.));
#5290=CARTESIAN_POINT('Ctrl Pts',(33.6743371481684,51.875,33.6743371481683));
#5291=CARTESIAN_POINT('Ctrl Pts',(23.,51.6666666666667,39.8371685740842));
#5292=CARTESIAN_POINT('Ctrl Pts',(13.9875081498766,51.4907679253478,45.0405331698222));
#5293=CARTESIAN_POINT('Ctrl Pts',(3.61292728433799,51.311710737147,45.8578974271399));
#5294=CARTESIAN_POINT('Origin',(0.,60.,0.));
#5295=CARTESIAN_POINT('',(45.7957082162897,47.5741208584476,-4.33048599679672));
#5296=CARTESIAN_POINT('',(45.7957082162897,48.1991208721035,-4.33048599679673));
#5297=CARTESIAN_POINT('',(45.7957082162897,60.,-4.33048599679673));
#5298=CARTESIAN_POINT('',(3.61292728433796,48.688289262853,-45.8578974271399));
#5299=CARTESIAN_POINT('Ctrl Pts',(3.61292728433796,48.688289262853,-45.8578974271399));
#5300=CARTESIAN_POINT('Ctrl Pts',(13.9875081498765,48.5092320746522,-45.0405331698222));
#5301=CARTESIAN_POINT('Ctrl Pts',(23.,48.3333333333333,-39.8371685740842));
#5302=CARTESIAN_POINT('Ctrl Pts',(33.6743371481683,48.125,-33.6743371481684));
#5303=CARTESIAN_POINT('Ctrl Pts',(39.8371685740842,47.9166666666667,-23.));
#5304=CARTESIAN_POINT('Ctrl Pts',(44.8515840435634,47.7471553142903,-14.3147776366027));
#5305=CARTESIAN_POINT('Ctrl Pts',(45.7957082162897,47.5741208584476,-4.33048599679672));
#5306=CARTESIAN_POINT('',(3.61292728433799,49.3132892765089,-45.8578974271399));
#5307=CARTESIAN_POINT('',(3.61292728433799,60.,-45.8578974271399));
#5308=CARTESIAN_POINT('Ctrl Pts',(3.61292728433799,49.3132892765089,-45.8578974271399));
#5309=CARTESIAN_POINT('Ctrl Pts',(13.9875081498766,49.1342320883081,-45.0405331698222));
#5310=CARTESIAN_POINT('Ctrl Pts',(23.,48.9583333469893,-39.8371685740842));
#5311=CARTESIAN_POINT('Ctrl Pts',(33.6743371481683,48.7500000136559,-33.6743371481684));
#5312=CARTESIAN_POINT('Ctrl Pts',(39.8371685740842,48.5416666803226,-23.));
#5313=CARTESIAN_POINT('Ctrl Pts',(44.8515840435634,48.3721553279462,-14.3147776366027));
#5314=CARTESIAN_POINT('Ctrl Pts',(45.7957082162897,48.1991208721035,-4.33048599679673));
#5315=CARTESIAN_POINT('Origin',(0.,60.,0.));
#5316=CARTESIAN_POINT('',(45.858362923034,48.0633913333999,3.60701400320327));
#5317=CARTESIAN_POINT('',(45.858362923034,47.438391319744,3.60701400320324));
#5318=CARTESIAN_POINT('',(45.858362923034,60.,3.60701400320327));
#5319=CARTESIAN_POINT('',(3.61292728433798,46.936710750803,45.8578974271399));
#5320=CARTESIAN_POINT('Ctrl Pts',(45.858362923034,48.0633913333999,3.60701400320327));
#5321=CARTESIAN_POINT('Ctrl Pts',(45.0420919829705,47.8842847836874,13.9848082063043));
#5322=CARTESIAN_POINT('Ctrl Pts',(39.8371685740842,47.7083333469893,23.));
#5323=CARTESIAN_POINT('Ctrl Pts',(33.6743371481684,47.5000000136559,33.6743371481683));
#5324=CARTESIAN_POINT('Ctrl Pts',(23.,47.2916666803226,39.8371685740842));
#5325=CARTESIAN_POINT('Ctrl Pts',(13.9875081498766,47.1157679390037,45.0405331698222));
#5326=CARTESIAN_POINT('Ctrl Pts',(3.61292728433798,46.9367107508029,45.8578974271399));
#5327=CARTESIAN_POINT('',(3.61292728433799,46.311710737147,45.8578974271399));
#5328=CARTESIAN_POINT('',(3.61292728433799,60.,45.8578974271399));
#5329=CARTESIAN_POINT('Ctrl Pts',(45.858362923034,47.438391319744,3.60701400320324));
#5330=CARTESIAN_POINT('Ctrl Pts',(45.0420919829705,47.2592847700314,13.9848082063043));
#5331=CARTESIAN_POINT('Ctrl Pts',(39.8371685740842,47.0833333333333,23.));
#5332=CARTESIAN_POINT('Ctrl Pts',(33.6743371481684,46.875,33.6743371481683));
#5333=CARTESIAN_POINT('Ctrl Pts',(23.,46.6666666666667,39.8371685740842));
#5334=CARTESIAN_POINT('Ctrl Pts',(13.9875081498766,46.4907679253478,45.0405331698222));
#5335=CARTESIAN_POINT('Ctrl Pts',(3.61292728433799,46.311710737147,45.8578974271399));
#5336=CARTESIAN_POINT('Origin',(0.,60.,0.));
#5337=CARTESIAN_POINT('',(45.7957082162897,42.5741208584476,-4.3304859967968));
#5338=CARTESIAN_POINT('',(45.7957082162897,43.1991208721035,-4.33048599679673));
#5339=CARTESIAN_POINT('',(45.7957082162897,60.,-4.33048599679673));
#5340=CARTESIAN_POINT('',(3.61292728433795,43.688289262853,-45.8578974271399));
#5341=CARTESIAN_POINT('Ctrl Pts',(3.61292728433794,43.688289262853,-45.8578974271399));
#5342=CARTESIAN_POINT('Ctrl Pts',(13.9875081498765,43.5092320746522,-45.0405331698223));
#5343=CARTESIAN_POINT('Ctrl Pts',(23.,43.3333333333333,-39.8371685740842));
#5344=CARTESIAN_POINT('Ctrl Pts',(33.6743371481683,43.125,-33.6743371481684));
#5345=CARTESIAN_POINT('Ctrl Pts',(39.8371685740842,42.9166666666667,-23.));
#5346=CARTESIAN_POINT('Ctrl Pts',(44.8515840435634,42.7471553142903,-14.3147776366027));
#5347=CARTESIAN_POINT('Ctrl Pts',(45.7957082162897,42.5741208584476,-4.3304859967968));
#5348=CARTESIAN_POINT('',(3.61292728433799,44.3132892765089,-45.8578974271399));
#5349=CARTESIAN_POINT('',(3.61292728433799,60.,-45.8578974271399));
#5350=CARTESIAN_POINT('Ctrl Pts',(3.61292728433799,44.3132892765089,-45.8578974271399));
#5351=CARTESIAN_POINT('Ctrl Pts',(13.9875081498766,44.1342320883081,-45.0405331698222));
#5352=CARTESIAN_POINT('Ctrl Pts',(23.,43.9583333469893,-39.8371685740842));
#5353=CARTESIAN_POINT('Ctrl Pts',(33.6743371481683,43.7500000136559,-33.6743371481684));
#5354=CARTESIAN_POINT('Ctrl Pts',(39.8371685740842,43.5416666803226,-23.));
#5355=CARTESIAN_POINT('Ctrl Pts',(44.8515840435634,43.3721553279462,-14.3147776366027));
#5356=CARTESIAN_POINT('Ctrl Pts',(45.7957082162897,43.1991208721035,-4.33048599679673));
#5357=CARTESIAN_POINT('Origin',(0.,60.,0.));
#5358=CARTESIAN_POINT('',(45.858362923034,43.0633913333999,3.60701400320327));
#5359=CARTESIAN_POINT('',(45.858362923034,42.438391319744,3.60701400320326));
#5360=CARTESIAN_POINT('',(45.858362923034,60.,3.60701400320327));
#5361=CARTESIAN_POINT('',(3.61292728433799,41.936710750803,45.8578974271399));
#5362=CARTESIAN_POINT('Ctrl Pts',(45.858362923034,43.0633913333999,3.60701400320327));
#5363=CARTESIAN_POINT('Ctrl Pts',(45.0420919829705,42.8842847836874,13.9848082063043));
#5364=CARTESIAN_POINT('Ctrl Pts',(39.8371685740842,42.7083333469893,23.));
#5365=CARTESIAN_POINT('Ctrl Pts',(33.6743371481684,42.5000000136559,33.6743371481683));
#5366=CARTESIAN_POINT('Ctrl Pts',(23.,42.2916666803226,39.8371685740842));
#5367=CARTESIAN_POINT('Ctrl Pts',(13.9875081498766,42.1157679390038,45.0405331698222));
#5368=CARTESIAN_POINT('Ctrl Pts',(3.61292728433799,41.936710750803,45.8578974271399));
#5369=CARTESIAN_POINT('',(3.61292728433799,41.311710737147,45.8578974271399));
#5370=CARTESIAN_POINT('',(3.61292728433799,60.,45.8578974271399));
#5371=CARTESIAN_POINT('Ctrl Pts',(45.858362923034,42.438391319744,3.60701400320326));
#5372=CARTESIAN_POINT('Ctrl Pts',(45.0420919829705,42.2592847700314,13.9848082063042));
#5373=CARTESIAN_POINT('Ctrl Pts',(39.8371685740842,42.0833333333333,23.));
#5374=CARTESIAN_POINT('Ctrl Pts',(33.6743371481684,41.875,33.6743371481683));
#5375=CARTESIAN_POINT('Ctrl Pts',(23.,41.6666666666667,39.8371685740842));
#5376=CARTESIAN_POINT('Ctrl Pts',(13.9875081498766,41.4907679253478,45.0405331698223));
#5377=CARTESIAN_POINT('Ctrl Pts',(3.61292728433799,41.311710737147,45.8578974271399));
#5378=CARTESIAN_POINT('Origin',(0.,60.,0.));
#5379=CARTESIAN_POINT('',(-45.7957082162897,55.5508791552084,-4.33048599679673));
#5380=CARTESIAN_POINT('',(-45.7957082162897,54.9258791415524,-4.33048599679671));
#5381=CARTESIAN_POINT('',(-45.7957082162897,60.,-4.33048599679673));
#5382=CARTESIAN_POINT('',(-4.32456003949879,54.4490181730497,-45.7962681936506));
#5383=CARTESIAN_POINT('Ctrl Pts',(-45.7957082162897,55.5508791552084,-4.33048599679673));
#5384=CARTESIAN_POINT('Ctrl Pts',(-44.8515840435634,55.3778446993657,-14.3147776366027));
#5385=CARTESIAN_POINT('Ctrl Pts',(-39.8371685740842,55.2083333469893,-23.));
#5386=CARTESIAN_POINT('Ctrl Pts',(-33.6743371481684,55.0000000136559,-33.6743371481684));
#5387=CARTESIAN_POINT('Ctrl Pts',(-23.,54.7916666803226,-39.8371685740842));
#5388=CARTESIAN_POINT('Ctrl Pts',(-14.3120776418265,54.6221026315676,-44.8531428862742));
#5389=CARTESIAN_POINT('Ctrl Pts',(-4.32456003949879,54.4490181730497,-45.7962681936506));
#5390=CARTESIAN_POINT('',(-4.32456003949879,53.8240181593938,-45.7962681936506));
#5391=CARTESIAN_POINT('',(-4.32456003949879,60.,-45.7962681936506));
#5392=CARTESIAN_POINT('Ctrl Pts',(-45.7957082162897,54.9258791415524,-4.33048599679671));
#5393=CARTESIAN_POINT('Ctrl Pts',(-44.8515840435634,54.7528446857097,-14.3147776366027));
#5394=CARTESIAN_POINT('Ctrl Pts',(-39.8371685740842,54.5833333333333,-23.));
#5395=CARTESIAN_POINT('Ctrl Pts',(-33.6743371481684,54.375,-33.6743371481684));
#5396=CARTESIAN_POINT('Ctrl Pts',(-23.,54.1666666666667,-39.8371685740842));
#5397=CARTESIAN_POINT('Ctrl Pts',(-14.3120776418265,53.9971026179117,-44.8531428862742));
#5398=CARTESIAN_POINT('Ctrl Pts',(-4.32456003949879,53.8240181593938,-45.7962681936506));
#5399=CARTESIAN_POINT('Origin',(0.,60.,0.));
#5400=CARTESIAN_POINT('',(-45.858362923034,55.061608680256,3.60701400320327));
#5401=CARTESIAN_POINT('',(-45.858362923034,57.,3.60701400320327));
#5402=CARTESIAN_POINT('',(-45.858362923034,60.,3.60701400320327));
#5403=CARTESIAN_POINT('',(-4.32456003949879,56.1759818406063,45.7962681936506));
#5404=CARTESIAN_POINT('Ctrl Pts',(-4.32456003949879,56.1759818406063,45.7962681936506));
#5405=CARTESIAN_POINT('Ctrl Pts',(-14.3120776418264,56.0028973820884,44.8531428862743));
#5406=CARTESIAN_POINT('Ctrl Pts',(-23.,55.8333333333333,39.8371685740842));
#5407=CARTESIAN_POINT('Ctrl Pts',(-33.6743371481683,55.625,33.6743371481684));
#5408=CARTESIAN_POINT('Ctrl Pts',(-39.8371685740842,55.4166666666667,23.));
#5409=CARTESIAN_POINT('Ctrl Pts',(-45.0420919829705,55.2407152299686,13.9848082063043));
#5410=CARTESIAN_POINT('Ctrl Pts',(-45.858362923034,55.061608680256,3.60701400320327));
#5411=CARTESIAN_POINT('',(-4.32456003949879,57.,45.7962681936506));
#5412=CARTESIAN_POINT('',(-4.32456003949879,60.,45.7962681936506));
#5413=CARTESIAN_POINT('Origin',(0.,57.,0.));
#5414=CARTESIAN_POINT('Origin',(0.,60.,0.));
#5415=CARTESIAN_POINT('',(-45.7957082162897,50.5508791552084,-4.33048599679673));
#5416=CARTESIAN_POINT('',(-45.7957082162897,49.9258791415524,-4.33048599679671));
#5417=CARTESIAN_POINT('',(-45.7957082162897,60.,-4.33048599679673));
#5418=CARTESIAN_POINT('',(-4.32456003949879,49.4490181730497,-45.7962681936506));
#5419=CARTESIAN_POINT('Ctrl Pts',(-45.7957082162897,50.5508791552084,-4.33048599679673));
#5420=CARTESIAN_POINT('Ctrl Pts',(-44.8515840435634,50.3778446993657,-14.3147776366027));
#5421=CARTESIAN_POINT('Ctrl Pts',(-39.8371685740842,50.2083333469893,-23.));
#5422=CARTESIAN_POINT('Ctrl Pts',(-33.6743371481684,50.0000000136559,-33.6743371481684));
#5423=CARTESIAN_POINT('Ctrl Pts',(-23.,49.7916666803226,-39.8371685740842));
#5424=CARTESIAN_POINT('Ctrl Pts',(-14.3120776418265,49.6221026315676,-44.8531428862742));
#5425=CARTESIAN_POINT('Ctrl Pts',(-4.32456003949879,49.4490181730497,-45.7962681936506));
#5426=CARTESIAN_POINT('',(-4.32456003949879,48.8240181593938,-45.7962681936506));
#5427=CARTESIAN_POINT('',(-4.32456003949879,60.,-45.7962681936506));
#5428=CARTESIAN_POINT('Ctrl Pts',(-45.7957082162897,49.9258791415524,-4.33048599679671));
#5429=CARTESIAN_POINT('Ctrl Pts',(-44.8515840435634,49.7528446857098,-14.3147776366027));
#5430=CARTESIAN_POINT('Ctrl Pts',(-39.8371685740842,49.5833333333333,-23.));
#5431=CARTESIAN_POINT('Ctrl Pts',(-33.6743371481684,49.375,-33.6743371481684));
#5432=CARTESIAN_POINT('Ctrl Pts',(-23.,49.1666666666667,-39.8371685740842));
#5433=CARTESIAN_POINT('Ctrl Pts',(-14.3120776418265,48.9971026179117,-44.8531428862742));
#5434=CARTESIAN_POINT('Ctrl Pts',(-4.32456003949879,48.8240181593938,-45.7962681936506));
#5435=CARTESIAN_POINT('Origin',(0.,60.,0.));
#5436=CARTESIAN_POINT('',(-45.858362923034,50.061608680256,3.60701400320326));
#5437=CARTESIAN_POINT('',(-45.858362923034,50.686608693912,3.60701400320327));
#5438=CARTESIAN_POINT('',(-45.858362923034,60.,3.60701400320327));
#5439=CARTESIAN_POINT('',(-4.32456003949879,51.1759818406062,45.7962681936506));
#5440=CARTESIAN_POINT('Ctrl Pts',(-4.32456003949879,51.1759818406063,45.7962681936506));
#5441=CARTESIAN_POINT('Ctrl Pts',(-14.3120776418264,51.0028973820884,44.8531428862743));
#5442=CARTESIAN_POINT('Ctrl Pts',(-23.,50.8333333333333,39.8371685740842));
#5443=CARTESIAN_POINT('Ctrl Pts',(-33.6743371481683,50.625,33.6743371481684));
#5444=CARTESIAN_POINT('Ctrl Pts',(-39.8371685740842,50.4166666666667,23.));
#5445=CARTESIAN_POINT('Ctrl Pts',(-45.0420919829705,50.2407152299686,13.9848082063043));
#5446=CARTESIAN_POINT('Ctrl Pts',(-45.858362923034,50.061608680256,3.60701400320326));
#5447=CARTESIAN_POINT('',(-4.32456003949877,51.8009818542622,45.7962681936506));
#5448=CARTESIAN_POINT('',(-4.32456003949879,60.,45.7962681936506));
#5449=CARTESIAN_POINT('Ctrl Pts',(-4.32456003949877,51.8009818542622,45.7962681936506));
#5450=CARTESIAN_POINT('Ctrl Pts',(-14.3120776418264,51.6278973957443,44.8531428862743));
#5451=CARTESIAN_POINT('Ctrl Pts',(-23.,51.4583333469893,39.8371685740842));
#5452=CARTESIAN_POINT('Ctrl Pts',(-33.6743371481683,51.2500000136559,33.6743371481684));
#5453=CARTESIAN_POINT('Ctrl Pts',(-39.8371685740842,51.0416666803226,23.));
#5454=CARTESIAN_POINT('Ctrl Pts',(-45.0420919829705,50.8657152436245,13.9848082063043));
#5455=CARTESIAN_POINT('Ctrl Pts',(-45.858362923034,50.686608693912,3.60701400320327));
#5456=CARTESIAN_POINT('Origin',(0.,60.,0.));
#5457=CARTESIAN_POINT('',(-45.7957082162897,45.5508791552084,-4.33048599679673));
#5458=CARTESIAN_POINT('',(-45.7957082162897,44.9258791415524,-4.33048599679682));
#5459=CARTESIAN_POINT('',(-45.7957082162897,60.,-4.33048599679673));
#5460=CARTESIAN_POINT('',(-4.32456003949874,44.4490181730497,-45.7962681936506));
#5461=CARTESIAN_POINT('Ctrl Pts',(-45.7957082162897,45.5508791552084,-4.33048599679673));
#5462=CARTESIAN_POINT('Ctrl Pts',(-44.8515840435634,45.3778446993657,-14.3147776366027));
#5463=CARTESIAN_POINT('Ctrl Pts',(-39.8371685740842,45.2083333469893,-23.));
#5464=CARTESIAN_POINT('Ctrl Pts',(-33.6743371481684,45.0000000136559,-33.6743371481684));
#5465=CARTESIAN_POINT('Ctrl Pts',(-23.,44.7916666803226,-39.8371685740842));
#5466=CARTESIAN_POINT('Ctrl Pts',(-14.3120776418264,44.6221026315676,-44.8531428862743));
#5467=CARTESIAN_POINT('Ctrl Pts',(-4.32456003949874,44.4490181730497,-45.7962681936506));
#5468=CARTESIAN_POINT('',(-4.32456003949879,43.8240181593938,-45.7962681936506));
#5469=CARTESIAN_POINT('',(-4.32456003949879,60.,-45.7962681936506));
#5470=CARTESIAN_POINT('Ctrl Pts',(-45.7957082162897,44.9258791415524,-4.33048599679682));
#5471=CARTESIAN_POINT('Ctrl Pts',(-44.8515840435634,44.7528446857097,-14.3147776366027));
#5472=CARTESIAN_POINT('Ctrl Pts',(-39.8371685740842,44.5833333333333,-23.));
#5473=CARTESIAN_POINT('Ctrl Pts',(-33.6743371481684,44.375,-33.6743371481684));
#5474=CARTESIAN_POINT('Ctrl Pts',(-23.,44.1666666666667,-39.8371685740842));
#5475=CARTESIAN_POINT('Ctrl Pts',(-14.3120776418264,43.9971026179117,-44.8531428862742));
#5476=CARTESIAN_POINT('Ctrl Pts',(-4.32456003949879,43.8240181593938,-45.7962681936506));
#5477=CARTESIAN_POINT('Origin',(0.,60.,0.));
#5478=CARTESIAN_POINT('',(-45.858362923034,45.061608680256,3.60701400320326));
#5479=CARTESIAN_POINT('',(-45.858362923034,45.686608693912,3.60701400320327));
#5480=CARTESIAN_POINT('',(-45.858362923034,60.,3.60701400320327));
#5481=CARTESIAN_POINT('',(-4.32456003949879,46.1759818406062,45.7962681936506));
#5482=CARTESIAN_POINT('Ctrl Pts',(-4.32456003949879,46.1759818406063,45.7962681936506));
#5483=CARTESIAN_POINT('Ctrl Pts',(-14.3120776418264,46.0028973820884,44.8531428862743));
#5484=CARTESIAN_POINT('Ctrl Pts',(-23.,45.8333333333333,39.8371685740842));
#5485=CARTESIAN_POINT('Ctrl Pts',(-33.6743371481683,45.625,33.6743371481684));
#5486=CARTESIAN_POINT('Ctrl Pts',(-39.8371685740842,45.4166666666667,23.));
#5487=CARTESIAN_POINT('Ctrl Pts',(-45.0420919829705,45.2407152299686,13.9848082063043));
#5488=CARTESIAN_POINT('Ctrl Pts',(-45.858362923034,45.0616086802561,3.60701400320326));
#5489=CARTESIAN_POINT('',(-4.32456003949882,46.8009818542622,45.7962681936506));
#5490=CARTESIAN_POINT('',(-4.32456003949879,60.,45.7962681936506));
#5491=CARTESIAN_POINT('Ctrl Pts',(-4.32456003949882,46.8009818542622,45.7962681936506));
#5492=CARTESIAN_POINT('Ctrl Pts',(-14.3120776418264,46.6278973957443,44.8531428862743));
#5493=CARTESIAN_POINT('Ctrl Pts',(-23.,46.4583333469893,39.8371685740842));
#5494=CARTESIAN_POINT('Ctrl Pts',(-33.6743371481683,46.2500000136559,33.6743371481684));
#5495=CARTESIAN_POINT('Ctrl Pts',(-39.8371685740842,46.0416666803226,23.));
#5496=CARTESIAN_POINT('Ctrl Pts',(-45.0420919829705,45.8657152436245,13.9848082063043));
#5497=CARTESIAN_POINT('Ctrl Pts',(-45.858362923034,45.686608693912,3.60701400320327));
#5498=CARTESIAN_POINT('Origin',(0.,60.,0.));
#5499=CARTESIAN_POINT('',(-45.7957082162897,40.5508791552084,-4.33048599679673));
#5500=CARTESIAN_POINT('',(-45.7957082162897,39.9258791415524,-4.33048599679679));
#5501=CARTESIAN_POINT('',(-45.7957082162897,60.,-4.33048599679673));
#5502=CARTESIAN_POINT('',(-4.32456003949876,39.4490181730497,-45.7962681936506));
#5503=CARTESIAN_POINT('Ctrl Pts',(-45.7957082162897,40.5508791552084,-4.33048599679673));
#5504=CARTESIAN_POINT('Ctrl Pts',(-44.8515840435634,40.3778446993657,-14.3147776366027));
#5505=CARTESIAN_POINT('Ctrl Pts',(-39.8371685740842,40.2083333469893,-23.));
#5506=CARTESIAN_POINT('Ctrl Pts',(-33.6743371481684,40.0000000136559,-33.6743371481684));
#5507=CARTESIAN_POINT('Ctrl Pts',(-23.,39.7916666803226,-39.8371685740842));
#5508=CARTESIAN_POINT('Ctrl Pts',(-14.3120776418264,39.6221026315676,-44.8531428862742));
#5509=CARTESIAN_POINT('Ctrl Pts',(-4.32456003949876,39.4490181730497,-45.7962681936506));
#5510=CARTESIAN_POINT('',(-4.32456003949879,38.8240181593937,-45.7962681936506));
#5511=CARTESIAN_POINT('',(-4.32456003949879,60.,-45.7962681936506));
#5512=CARTESIAN_POINT('Ctrl Pts',(-45.7957082162897,39.9258791415524,-4.33048599679679));
#5513=CARTESIAN_POINT('Ctrl Pts',(-44.8515840435634,39.7528446857097,-14.3147776366027));
#5514=CARTESIAN_POINT('Ctrl Pts',(-39.8371685740842,39.5833333333333,-23.));
#5515=CARTESIAN_POINT('Ctrl Pts',(-33.6743371481684,39.375,-33.6743371481684));
#5516=CARTESIAN_POINT('Ctrl Pts',(-23.,39.1666666666667,-39.8371685740842));
#5517=CARTESIAN_POINT('Ctrl Pts',(-14.3120776418264,38.9971026179116,-44.8531428862743));
#5518=CARTESIAN_POINT('Ctrl Pts',(-4.32456003949879,38.8240181593937,-45.7962681936506));
#5519=CARTESIAN_POINT('Origin',(0.,60.,0.));
#5520=CARTESIAN_POINT('',(-45.858362923034,40.061608680256,3.60701400320328));
#5521=CARTESIAN_POINT('',(-45.858362923034,40.686608693912,3.60701400320327));
#5522=CARTESIAN_POINT('',(-45.858362923034,60.,3.60701400320327));
#5523=CARTESIAN_POINT('',(-4.32456003949879,41.1759818406062,45.7962681936506));
#5524=CARTESIAN_POINT('Ctrl Pts',(-4.32456003949879,41.1759818406063,45.7962681936506));
#5525=CARTESIAN_POINT('Ctrl Pts',(-14.3120776418264,41.0028973820884,44.8531428862743));
#5526=CARTESIAN_POINT('Ctrl Pts',(-23.,40.8333333333333,39.8371685740842));
#5527=CARTESIAN_POINT('Ctrl Pts',(-33.6743371481683,40.625,33.6743371481684));
#5528=CARTESIAN_POINT('Ctrl Pts',(-39.8371685740842,40.4166666666667,23.));
#5529=CARTESIAN_POINT('Ctrl Pts',(-45.0420919829705,40.2407152299686,13.9848082063043));
#5530=CARTESIAN_POINT('Ctrl Pts',(-45.858362923034,40.061608680256,3.60701400320328));
#5531=CARTESIAN_POINT('',(-4.32456003949882,41.8009818542622,45.7962681936506));
#5532=CARTESIAN_POINT('',(-4.32456003949879,60.,45.7962681936506));
#5533=CARTESIAN_POINT('Ctrl Pts',(-4.32456003949882,41.8009818542622,45.7962681936506));
#5534=CARTESIAN_POINT('Ctrl Pts',(-14.3120776418264,41.6278973957443,44.8531428862743));
#5535=CARTESIAN_POINT('Ctrl Pts',(-23.,41.4583333469893,39.8371685740842));
#5536=CARTESIAN_POINT('Ctrl Pts',(-33.6743371481683,41.2500000136559,33.6743371481684));
#5537=CARTESIAN_POINT('Ctrl Pts',(-39.8371685740842,41.0416666803226,23.));
#5538=CARTESIAN_POINT('Ctrl Pts',(-45.0420919829705,40.8657152436245,13.9848082063043));
#5539=CARTESIAN_POINT('Ctrl Pts',(-45.858362923034,40.686608693912,3.60701400320327));
#5540=CARTESIAN_POINT('Ctrl Pts',(-46.,55.6250000136559,0.));
#5541=CARTESIAN_POINT('Ctrl Pts',(-46.,55.4166666803226,-12.3256628518316));
#5542=CARTESIAN_POINT('Ctrl Pts',(-39.8371685740842,55.2083333469893,-23.));
#5543=CARTESIAN_POINT('Ctrl Pts',(-33.6743371481684,55.0000000136559,-33.6743371481684));
#5544=CARTESIAN_POINT('Ctrl Pts',(-23.,54.7916666803226,-39.8371685740842));
#5545=CARTESIAN_POINT('Ctrl Pts',(-12.3256628518317,54.5833333469893,-46.));
#5546=CARTESIAN_POINT('Ctrl Pts',(-2.81668763803891E-15,54.3750000136559,
-46.));
#5547=CARTESIAN_POINT('Ctrl Pts',(12.3256628518316,54.1666666803226,-46.));
#5548=CARTESIAN_POINT('Ctrl Pts',(23.,53.9583333469893,-39.8371685740842));
#5549=CARTESIAN_POINT('Ctrl Pts',(33.6743371481683,53.7500000136559,-33.6743371481684));
#5550=CARTESIAN_POINT('Ctrl Pts',(39.8371685740842,53.5416666803226,-23.));
#5551=CARTESIAN_POINT('Ctrl Pts',(46.,53.3333333469893,-12.3256628518317));
#5552=CARTESIAN_POINT('Ctrl Pts',(46.,53.1250000136559,-5.63337527607782E-15));
#5553=CARTESIAN_POINT('Ctrl Pts',(46.,52.9166666803226,12.3256628518316));
#5554=CARTESIAN_POINT('Ctrl Pts',(39.8371685740842,52.7083333469893,23.));
#5555=CARTESIAN_POINT('Ctrl Pts',(33.6743371481684,52.5000000136559,33.6743371481683));
#5556=CARTESIAN_POINT('Ctrl Pts',(23.,52.2916666803226,39.8371685740842));
#5557=CARTESIAN_POINT('Ctrl Pts',(12.3256628518317,52.0833333469893,46.));
#5558=CARTESIAN_POINT('Ctrl Pts',(8.45006291411674E-15,51.8750000136559,
46.));
#5559=CARTESIAN_POINT('Ctrl Pts',(-12.3256628518316,51.6666666803226,46.));
#5560=CARTESIAN_POINT('Ctrl Pts',(-23.,51.4583333469893,39.8371685740842));
#5561=CARTESIAN_POINT('Ctrl Pts',(-33.6743371481683,51.2500000136559,33.6743371481684));
#5562=CARTESIAN_POINT('Ctrl Pts',(-39.8371685740842,51.0416666803226,23.));
#5563=CARTESIAN_POINT('Ctrl Pts',(-46.,50.8333333469893,12.3256628518317));
#5564=CARTESIAN_POINT('Ctrl Pts',(-46.,50.6250000136559,0.));
#5565=CARTESIAN_POINT('Ctrl Pts',(-46.,50.4166666803226,-12.3256628518316));
#5566=CARTESIAN_POINT('Ctrl Pts',(-39.8371685740842,50.2083333469893,-23.));
#5567=CARTESIAN_POINT('Ctrl Pts',(-33.6743371481684,50.0000000136559,-33.6743371481684));
#5568=CARTESIAN_POINT('Ctrl Pts',(-23.,49.7916666803226,-39.8371685740842));
#5569=CARTESIAN_POINT('Ctrl Pts',(-12.3256628518317,49.5833333469893,-46.));
#5570=CARTESIAN_POINT('Ctrl Pts',(-2.81668763803891E-15,49.3750000136559,
-46.));
#5571=CARTESIAN_POINT('Ctrl Pts',(12.3256628518316,49.1666666803226,-46.));
#5572=CARTESIAN_POINT('Ctrl Pts',(23.,48.9583333469893,-39.8371685740842));
#5573=CARTESIAN_POINT('Ctrl Pts',(33.6743371481683,48.7500000136559,-33.6743371481684));
#5574=CARTESIAN_POINT('Ctrl Pts',(39.8371685740842,48.5416666803226,-23.));
#5575=CARTESIAN_POINT('Ctrl Pts',(46.,48.3333333469893,-12.3256628518317));
#5576=CARTESIAN_POINT('Ctrl Pts',(46.,48.1250000136559,-5.63337527607782E-15));
#5577=CARTESIAN_POINT('Ctrl Pts',(46.,47.9166666803226,12.3256628518316));
#5578=CARTESIAN_POINT('Ctrl Pts',(39.8371685740842,47.7083333469893,23.));
#5579=CARTESIAN_POINT('Ctrl Pts',(33.6743371481684,47.5000000136559,33.6743371481683));
#5580=CARTESIAN_POINT('Ctrl Pts',(23.,47.2916666803226,39.8371685740842));
#5581=CARTESIAN_POINT('Ctrl Pts',(12.3256628518317,47.0833333469893,46.));
#5582=CARTESIAN_POINT('Ctrl Pts',(8.45006291411674E-15,46.8750000136559,
46.));
#5583=CARTESIAN_POINT('Ctrl Pts',(-12.3256628518316,46.6666666803226,46.));
#5584=CARTESIAN_POINT('Ctrl Pts',(-23.,46.4583333469893,39.8371685740842));
#5585=CARTESIAN_POINT('Ctrl Pts',(-33.6743371481683,46.2500000136559,33.6743371481684));
#5586=CARTESIAN_POINT('Ctrl Pts',(-39.8371685740842,46.0416666803226,23.));
#5587=CARTESIAN_POINT('Ctrl Pts',(-46.,45.8333333469892,12.3256628518317));
#5588=CARTESIAN_POINT('Ctrl Pts',(-46.,45.6250000136559,0.));
#5589=CARTESIAN_POINT('Ctrl Pts',(-46.,45.4166666803226,-12.3256628518316));
#5590=CARTESIAN_POINT('Ctrl Pts',(-39.8371685740842,45.2083333469893,-23.));
#5591=CARTESIAN_POINT('Ctrl Pts',(-33.6743371481684,45.0000000136559,-33.6743371481684));
#5592=CARTESIAN_POINT('Ctrl Pts',(-23.,44.7916666803226,-39.8371685740842));
#5593=CARTESIAN_POINT('Ctrl Pts',(-12.3256628518317,44.5833333469893,-46.));
#5594=CARTESIAN_POINT('Ctrl Pts',(-2.81668763803891E-15,44.3750000136559,
-46.));
#5595=CARTESIAN_POINT('Ctrl Pts',(12.3256628518316,44.1666666803226,-46.));
#5596=CARTESIAN_POINT('Ctrl Pts',(23.,43.9583333469893,-39.8371685740842));
#5597=CARTESIAN_POINT('Ctrl Pts',(33.6743371481683,43.7500000136559,-33.6743371481684));
#5598=CARTESIAN_POINT('Ctrl Pts',(39.8371685740842,43.5416666803226,-23.));
#5599=CARTESIAN_POINT('Ctrl Pts',(46.,43.3333333469893,-12.3256628518317));
#5600=CARTESIAN_POINT('Ctrl Pts',(46.,43.1250000136559,-5.63337527607782E-15));
#5601=CARTESIAN_POINT('Ctrl Pts',(46.,42.9166666803226,12.3256628518316));
#5602=CARTESIAN_POINT('Ctrl Pts',(39.8371685740842,42.7083333469893,23.));
#5603=CARTESIAN_POINT('Ctrl Pts',(33.6743371481684,42.5000000136559,33.6743371481683));
#5604=CARTESIAN_POINT('Ctrl Pts',(23.,42.2916666803226,39.8371685740842));
#5605=CARTESIAN_POINT('Ctrl Pts',(12.3256628518317,42.0833333469893,46.));
#5606=CARTESIAN_POINT('Ctrl Pts',(8.45006291411674E-15,41.8750000136559,
46.));
#5607=CARTESIAN_POINT('Ctrl Pts',(-12.3256628518316,41.6666666803226,46.));
#5608=CARTESIAN_POINT('Ctrl Pts',(-23.,41.4583333469893,39.8371685740842));
#5609=CARTESIAN_POINT('Ctrl Pts',(-33.6743371481683,41.2500000136559,33.6743371481684));
#5610=CARTESIAN_POINT('Ctrl Pts',(-39.8371685740842,41.0416666803226,23.));
#5611=CARTESIAN_POINT('Ctrl Pts',(-46.,40.8333333469893,12.3256628518317));
#5612=CARTESIAN_POINT('Ctrl Pts',(-46.,40.6250000136559,0.));
#5613=CARTESIAN_POINT('Ctrl Pts',(-46.,40.4166666803226,-12.3256628518316));
#5614=CARTESIAN_POINT('Ctrl Pts',(-39.8371685740842,40.2083333469893,-23.));
#5615=CARTESIAN_POINT('Ctrl Pts',(-33.6743371481684,40.0000000136559,-33.6743371481684));
#5616=CARTESIAN_POINT('Ctrl Pts',(-23.,39.7916666803226,-39.8371685740842));
#5617=CARTESIAN_POINT('Ctrl Pts',(-12.3256628518317,39.5833333469893,-46.));
#5618=CARTESIAN_POINT('Ctrl Pts',(-2.81668763803891E-15,39.3750000136559,
-46.));
#5619=CARTESIAN_POINT('Ctrl Pts',(12.3256628518316,39.1666666803226,-46.));
#5620=CARTESIAN_POINT('Ctrl Pts',(23.,38.9583333469893,-39.8371685740842));
#5621=CARTESIAN_POINT('Ctrl Pts',(33.6743371481683,38.7500000136559,-33.6743371481684));
#5622=CARTESIAN_POINT('Ctrl Pts',(39.8371685740842,38.5416666803226,-23.));
#5623=CARTESIAN_POINT('Ctrl Pts',(46.,38.3333333469893,-12.3256628518317));
#5624=CARTESIAN_POINT('Ctrl Pts',(46.,38.1250000136559,-5.63337527607782E-15));
#5625=CARTESIAN_POINT('Ctrl Pts',(46.,37.9166666803226,12.3256628518316));
#5626=CARTESIAN_POINT('Ctrl Pts',(39.8371685740842,37.7083333469893,23.));
#5627=CARTESIAN_POINT('Ctrl Pts',(33.6743371481684,37.5000000136559,33.6743371481683));
#5628=CARTESIAN_POINT('Ctrl Pts',(23.,37.2916666803226,39.8371685740842));
#5629=CARTESIAN_POINT('Ctrl Pts',(12.3256628518317,37.0833333469893,46.));
#5630=CARTESIAN_POINT('Ctrl Pts',(8.45006291411674E-15,36.8750000136559,
46.));
#5631=CARTESIAN_POINT('Ctrl Pts',(-12.3256628518316,36.6666666803226,46.));
#5632=CARTESIAN_POINT('Ctrl Pts',(-23.,36.4583333469893,39.8371685740842));
#5633=CARTESIAN_POINT('Ctrl Pts',(-33.6743371481683,36.2500000136559,33.6743371481684));
#5634=CARTESIAN_POINT('Ctrl Pts',(-39.8371685740842,36.0416666803226,23.));
#5635=CARTESIAN_POINT('Ctrl Pts',(-46.,35.8333333469893,12.3256628518317));
#5636=CARTESIAN_POINT('Ctrl Pts',(-46.,35.6250000136559,0.));
#5637=CARTESIAN_POINT('Ctrl Pts',(-46.,35.4166666803226,-12.3256628518316));
#5638=CARTESIAN_POINT('Ctrl Pts',(-39.8371685740842,35.2083333469893,-23.));
#5639=CARTESIAN_POINT('Ctrl Pts',(-33.6743371481684,35.0000000136559,-33.6743371481684));
#5640=CARTESIAN_POINT('Ctrl Pts',(-23.,34.7916666803226,-39.8371685740842));
#5641=CARTESIAN_POINT('Ctrl Pts',(-12.3256628518317,34.5833333469893,-46.));
#5642=CARTESIAN_POINT('Ctrl Pts',(-2.81668763803891E-15,34.3750000136559,
-46.));
#5643=CARTESIAN_POINT('Ctrl Pts',(12.3256628518316,34.1666666803226,-46.));
#5644=CARTESIAN_POINT('Ctrl Pts',(23.,33.9583333469893,-39.8371685740842));
#5645=CARTESIAN_POINT('Ctrl Pts',(33.6743371481683,33.7500000136559,-33.6743371481684));
#5646=CARTESIAN_POINT('Ctrl Pts',(39.8371685740842,33.5416666803226,-23.));
#5647=CARTESIAN_POINT('Ctrl Pts',(46.,33.3333333469893,-12.3256628518317));
#5648=CARTESIAN_POINT('Ctrl Pts',(46.,33.1250000136559,-5.63337527607782E-15));
#5649=CARTESIAN_POINT('Ctrl Pts',(46.,32.9166666803226,12.3256628518316));
#5650=CARTESIAN_POINT('Ctrl Pts',(39.8371685740842,32.7083333469893,23.));
#5651=CARTESIAN_POINT('Ctrl Pts',(33.6743371481684,32.5000000136559,33.6743371481683));
#5652=CARTESIAN_POINT('Ctrl Pts',(23.,32.2916666803226,39.8371685740842));
#5653=CARTESIAN_POINT('Ctrl Pts',(12.3256628518317,32.0833333469893,46.));
#5654=CARTESIAN_POINT('Ctrl Pts',(8.45006291411674E-15,31.8750000136559,
46.));
#5655=CARTESIAN_POINT('Ctrl Pts',(-12.3256628518316,31.6666666803226,46.));
#5656=CARTESIAN_POINT('Ctrl Pts',(-23.,31.4583333469893,39.8371685740842));
#5657=CARTESIAN_POINT('Ctrl Pts',(-33.6743371481683,31.2500000136559,33.6743371481684));
#5658=CARTESIAN_POINT('Ctrl Pts',(-39.8371685740842,31.0416666803226,23.));
#5659=CARTESIAN_POINT('Ctrl Pts',(-46.,30.8333333469893,12.3256628518317));
#5660=CARTESIAN_POINT('Ctrl Pts',(-46.,30.6250000136559,0.));
#5661=CARTESIAN_POINT('Ctrl Pts',(-46.,30.4166666803226,-12.3256628518316));
#5662=CARTESIAN_POINT('Ctrl Pts',(-39.8371685740842,30.2083333469893,-23.));
#5663=CARTESIAN_POINT('Ctrl Pts',(-33.6743371481684,30.0000000136559,-33.6743371481684));
#5664=CARTESIAN_POINT('Ctrl Pts',(-23.,29.7916666803226,-39.8371685740842));
#5665=CARTESIAN_POINT('Ctrl Pts',(-12.3256628518317,29.5833333469893,-46.));
#5666=CARTESIAN_POINT('Ctrl Pts',(-2.81668763803891E-15,29.3750000136559,
-46.));
#5667=CARTESIAN_POINT('Ctrl Pts',(12.3256628518316,29.1666666803226,-46.));
#5668=CARTESIAN_POINT('Ctrl Pts',(23.,28.9583333469893,-39.8371685740842));
#5669=CARTESIAN_POINT('Ctrl Pts',(33.6743371481683,28.7500000136559,-33.6743371481684));
#5670=CARTESIAN_POINT('Ctrl Pts',(39.8371685740842,28.5416666803226,-23.));
#5671=CARTESIAN_POINT('Ctrl Pts',(46.,28.3333333469893,-12.3256628518317));
#5672=CARTESIAN_POINT('Ctrl Pts',(46.,28.1250000136559,-5.63337527607782E-15));
#5673=CARTESIAN_POINT('Ctrl Pts',(46.,27.9166666803226,12.3256628518316));
#5674=CARTESIAN_POINT('Ctrl Pts',(39.8371685740842,27.7083333469893,23.));
#5675=CARTESIAN_POINT('Ctrl Pts',(33.6743371481684,27.5000000136559,33.6743371481683));
#5676=CARTESIAN_POINT('Ctrl Pts',(23.,27.2916666803226,39.8371685740842));
#5677=CARTESIAN_POINT('Ctrl Pts',(12.3256628518317,27.0833333469893,46.));
#5678=CARTESIAN_POINT('Ctrl Pts',(8.45006291411674E-15,26.8750000136559,
46.));
#5679=CARTESIAN_POINT('Ctrl Pts',(-12.3256628518316,26.6666666803226,46.));
#5680=CARTESIAN_POINT('Ctrl Pts',(-23.,26.4583333469893,39.8371685740842));
#5681=CARTESIAN_POINT('Ctrl Pts',(-33.6743371481683,26.2500000136559,33.6743371481684));
#5682=CARTESIAN_POINT('Ctrl Pts',(-39.8371685740842,26.0416666803226,23.));
#5683=CARTESIAN_POINT('Ctrl Pts',(-46.,25.8333333469893,12.3256628518317));
#5684=CARTESIAN_POINT('Ctrl Pts',(-46.,25.6250000136559,0.));
#5685=CARTESIAN_POINT('Ctrl Pts',(-48.706329375,57.187500006828,-1.8898197019151E-14));
#5686=CARTESIAN_POINT('Ctrl Pts',(-48.706329375,56.9791666734946,-13.0508216223155));
#5687=CARTESIAN_POINT('Ctrl Pts',(-42.1809185638422,56.7708333401613,-24.3531646875));
#5688=CARTESIAN_POINT('Ctrl Pts',(-35.6555077526845,56.562500006828,-35.6555077526845));
#5689=CARTESIAN_POINT('Ctrl Pts',(-24.3531646875,56.3541666734946,-42.1809185638423));
#5690=CARTESIAN_POINT('Ctrl Pts',(-13.0508216223155,56.1458333401613,-48.706329375));
#5691=CARTESIAN_POINT('Ctrl Pts',(1.59157945007855E-14,55.937500006828,
-48.706329375));
#5692=CARTESIAN_POINT('Ctrl Pts',(13.0508216223155,55.7291666734946,-48.706329375));
#5693=CARTESIAN_POINT('Ctrl Pts',(24.3531646875,55.5208333401613,-42.1809185638422));
#5694=CARTESIAN_POINT('Ctrl Pts',(35.6555077526845,55.312500006828,-35.6555077526845));
#5695=CARTESIAN_POINT('Ctrl Pts',(42.1809185638422,55.1041666734946,-24.3531646875));
#5696=CARTESIAN_POINT('Ctrl Pts',(48.706329375,54.8958333401613,-13.0508216223155));
#5697=CARTESIAN_POINT('Ctrl Pts',(48.706329375,54.687500006828,1.293339198242E-14));
#5698=CARTESIAN_POINT('Ctrl Pts',(48.706329375,54.4791666734946,13.0508216223155));
#5699=CARTESIAN_POINT('Ctrl Pts',(42.1809185638422,54.2708333401613,24.3531646875));
#5700=CARTESIAN_POINT('Ctrl Pts',(35.6555077526845,54.062500006828,35.6555077526845));
#5701=CARTESIAN_POINT('Ctrl Pts',(24.3531646875,53.8541666734946,42.1809185638422));
#5702=CARTESIAN_POINT('Ctrl Pts',(13.0508216223155,53.6458333401613,48.706329375));
#5703=CARTESIAN_POINT('Ctrl Pts',(-9.95098946405443E-15,53.437500006828,
48.706329375));
#5704=CARTESIAN_POINT('Ctrl Pts',(-13.0508216223155,53.2291666734946,48.706329375));
#5705=CARTESIAN_POINT('Ctrl Pts',(-24.3531646875,53.0208333401613,42.1809185638423));
#5706=CARTESIAN_POINT('Ctrl Pts',(-35.6555077526845,52.812500006828,35.6555077526845));
#5707=CARTESIAN_POINT('Ctrl Pts',(-42.1809185638422,52.6041666734946,24.3531646875));
#5708=CARTESIAN_POINT('Ctrl Pts',(-48.706329375,52.3958333401613,13.0508216223155));
#5709=CARTESIAN_POINT('Ctrl Pts',(-48.706329375,52.187500006828,-1.8898197019151E-14));
#5710=CARTESIAN_POINT('Ctrl Pts',(-48.706329375,51.9791666734946,-13.0508216223155));
#5711=CARTESIAN_POINT('Ctrl Pts',(-42.1809185638422,51.7708333401613,-24.3531646875));
#5712=CARTESIAN_POINT('Ctrl Pts',(-35.6555077526845,51.562500006828,-35.6555077526845));
#5713=CARTESIAN_POINT('Ctrl Pts',(-24.3531646875,51.3541666734946,-42.1809185638423));
#5714=CARTESIAN_POINT('Ctrl Pts',(-13.0508216223155,51.1458333401613,-48.706329375));
#5715=CARTESIAN_POINT('Ctrl Pts',(1.59157945007855E-14,50.937500006828,
-48.706329375));
#5716=CARTESIAN_POINT('Ctrl Pts',(13.0508216223155,50.7291666734946,-48.706329375));
#5717=CARTESIAN_POINT('Ctrl Pts',(24.3531646875,50.5208333401613,-42.1809185638422));
#5718=CARTESIAN_POINT('Ctrl Pts',(35.6555077526845,50.312500006828,-35.6555077526845));
#5719=CARTESIAN_POINT('Ctrl Pts',(42.1809185638422,50.1041666734946,-24.3531646875));
#5720=CARTESIAN_POINT('Ctrl Pts',(48.706329375,49.8958333401613,-13.0508216223155));
#5721=CARTESIAN_POINT('Ctrl Pts',(48.706329375,49.687500006828,1.293339198242E-14));
#5722=CARTESIAN_POINT('Ctrl Pts',(48.706329375,49.4791666734946,13.0508216223155));
#5723=CARTESIAN_POINT('Ctrl Pts',(42.1809185638422,49.2708333401613,24.3531646875));
#5724=CARTESIAN_POINT('Ctrl Pts',(35.6555077526845,49.062500006828,35.6555077526845));
#5725=CARTESIAN_POINT('Ctrl Pts',(24.3531646875,48.8541666734946,42.1809185638422));
#5726=CARTESIAN_POINT('Ctrl Pts',(13.0508216223155,48.6458333401613,48.706329375));
#5727=CARTESIAN_POINT('Ctrl Pts',(-9.95098946405443E-15,48.437500006828,
48.706329375));
#5728=CARTESIAN_POINT('Ctrl Pts',(-13.0508216223155,48.2291666734946,48.706329375));
#5729=CARTESIAN_POINT('Ctrl Pts',(-24.3531646875,48.0208333401613,42.1809185638423));
#5730=CARTESIAN_POINT('Ctrl Pts',(-35.6555077526845,47.812500006828,35.6555077526845));
#5731=CARTESIAN_POINT('Ctrl Pts',(-42.1809185638422,47.6041666734946,24.3531646875));
#5732=CARTESIAN_POINT('Ctrl Pts',(-48.706329375,47.3958333401613,13.0508216223155));
#5733=CARTESIAN_POINT('Ctrl Pts',(-48.706329375,47.187500006828,-1.8898197019151E-14));
#5734=CARTESIAN_POINT('Ctrl Pts',(-48.706329375,46.9791666734946,-13.0508216223155));
#5735=CARTESIAN_POINT('Ctrl Pts',(-42.1809185638422,46.7708333401613,-24.3531646875));
#5736=CARTESIAN_POINT('Ctrl Pts',(-35.6555077526845,46.562500006828,-35.6555077526845));
#5737=CARTESIAN_POINT('Ctrl Pts',(-24.3531646875,46.3541666734946,-42.1809185638423));
#5738=CARTESIAN_POINT('Ctrl Pts',(-13.0508216223155,46.1458333401613,-48.706329375));
#5739=CARTESIAN_POINT('Ctrl Pts',(1.59157945007855E-14,45.937500006828,
-48.706329375));
#5740=CARTESIAN_POINT('Ctrl Pts',(13.0508216223155,45.7291666734946,-48.706329375));
#5741=CARTESIAN_POINT('Ctrl Pts',(24.3531646875,45.5208333401613,-42.1809185638422));
#5742=CARTESIAN_POINT('Ctrl Pts',(35.6555077526845,45.312500006828,-35.6555077526845));
#5743=CARTESIAN_POINT('Ctrl Pts',(42.1809185638422,45.1041666734946,-24.3531646875));
#5744=CARTESIAN_POINT('Ctrl Pts',(48.706329375,44.8958333401613,-13.0508216223155));
#5745=CARTESIAN_POINT('Ctrl Pts',(48.706329375,44.687500006828,1.293339198242E-14));
#5746=CARTESIAN_POINT('Ctrl Pts',(48.706329375,44.4791666734946,13.0508216223155));
#5747=CARTESIAN_POINT('Ctrl Pts',(42.1809185638422,44.2708333401613,24.3531646875));
#5748=CARTESIAN_POINT('Ctrl Pts',(35.6555077526845,44.062500006828,35.6555077526845));
#5749=CARTESIAN_POINT('Ctrl Pts',(24.3531646875,43.8541666734946,42.1809185638422));
#5750=CARTESIAN_POINT('Ctrl Pts',(13.0508216223155,43.6458333401613,48.706329375));
#5751=CARTESIAN_POINT('Ctrl Pts',(-9.95098946405443E-15,43.437500006828,
48.706329375));
#5752=CARTESIAN_POINT('Ctrl Pts',(-13.0508216223155,43.2291666734946,48.706329375));
#5753=CARTESIAN_POINT('Ctrl Pts',(-24.3531646875,43.0208333401613,42.1809185638423));
#5754=CARTESIAN_POINT('Ctrl Pts',(-35.6555077526845,42.812500006828,35.6555077526845));
#5755=CARTESIAN_POINT('Ctrl Pts',(-42.1809185638422,42.6041666734946,24.3531646875));
#5756=CARTESIAN_POINT('Ctrl Pts',(-48.706329375,42.3958333401613,13.0508216223155));
#5757=CARTESIAN_POINT('Ctrl Pts',(-48.706329375,42.187500006828,-1.8898197019151E-14));
#5758=CARTESIAN_POINT('Ctrl Pts',(-48.706329375,41.9791666734946,-13.0508216223155));
#5759=CARTESIAN_POINT('Ctrl Pts',(-42.1809185638422,41.7708333401613,-24.3531646875));
#5760=CARTESIAN_POINT('Ctrl Pts',(-35.6555077526845,41.562500006828,-35.6555077526845));
#5761=CARTESIAN_POINT('Ctrl Pts',(-24.3531646875,41.3541666734946,-42.1809185638423));
#5762=CARTESIAN_POINT('Ctrl Pts',(-13.0508216223155,41.1458333401613,-48.706329375));
#5763=CARTESIAN_POINT('Ctrl Pts',(1.59157945007855E-14,40.937500006828,
-48.706329375));
#5764=CARTESIAN_POINT('Ctrl Pts',(13.0508216223155,40.7291666734946,-48.706329375));
#5765=CARTESIAN_POINT('Ctrl Pts',(24.3531646875,40.5208333401613,-42.1809185638422));
#5766=CARTESIAN_POINT('Ctrl Pts',(35.6555077526845,40.312500006828,-35.6555077526845));
#5767=CARTESIAN_POINT('Ctrl Pts',(42.1809185638422,40.1041666734946,-24.3531646875));
#5768=CARTESIAN_POINT('Ctrl Pts',(48.706329375,39.8958333401613,-13.0508216223155));
#5769=CARTESIAN_POINT('Ctrl Pts',(48.706329375,39.687500006828,1.293339198242E-14));
#5770=CARTESIAN_POINT('Ctrl Pts',(48.706329375,39.4791666734946,13.0508216223155));
#5771=CARTESIAN_POINT('Ctrl Pts',(42.1809185638422,39.2708333401613,24.3531646875));
#5772=CARTESIAN_POINT('Ctrl Pts',(35.6555077526845,39.062500006828,35.6555077526845));
#5773=CARTESIAN_POINT('Ctrl Pts',(24.3531646875,38.8541666734946,42.1809185638422));
#5774=CARTESIAN_POINT('Ctrl Pts',(13.0508216223155,38.6458333401613,48.706329375));
#5775=CARTESIAN_POINT('Ctrl Pts',(-9.95098946405443E-15,38.437500006828,
48.706329375));
#5776=CARTESIAN_POINT('Ctrl Pts',(-13.0508216223155,38.2291666734946,48.706329375));
#5777=CARTESIAN_POINT('Ctrl Pts',(-24.3531646875,38.0208333401613,42.1809185638423));
#5778=CARTESIAN_POINT('Ctrl Pts',(-35.6555077526845,37.812500006828,35.6555077526845));
#5779=CARTESIAN_POINT('Ctrl Pts',(-42.1809185638422,37.6041666734946,24.3531646875));
#5780=CARTESIAN_POINT('Ctrl Pts',(-48.706329375,37.3958333401613,13.0508216223155));
#5781=CARTESIAN_POINT('Ctrl Pts',(-48.706329375,37.187500006828,-1.8898197019151E-14));
#5782=CARTESIAN_POINT('Ctrl Pts',(-48.706329375,36.9791666734946,-13.0508216223155));
#5783=CARTESIAN_POINT('Ctrl Pts',(-42.1809185638422,36.7708333401613,-24.3531646875));
#5784=CARTESIAN_POINT('Ctrl Pts',(-35.6555077526845,36.562500006828,-35.6555077526845));
#5785=CARTESIAN_POINT('Ctrl Pts',(-24.3531646875,36.3541666734946,-42.1809185638423));
#5786=CARTESIAN_POINT('Ctrl Pts',(-13.0508216223155,36.1458333401613,-48.706329375));
#5787=CARTESIAN_POINT('Ctrl Pts',(1.59157945007855E-14,35.937500006828,
-48.706329375));
#5788=CARTESIAN_POINT('Ctrl Pts',(13.0508216223155,35.7291666734946,-48.706329375));
#5789=CARTESIAN_POINT('Ctrl Pts',(24.3531646875,35.5208333401613,-42.1809185638422));
#5790=CARTESIAN_POINT('Ctrl Pts',(35.6555077526845,35.312500006828,-35.6555077526845));
#5791=CARTESIAN_POINT('Ctrl Pts',(42.1809185638422,35.1041666734946,-24.3531646875));
#5792=CARTESIAN_POINT('Ctrl Pts',(48.706329375,34.8958333401613,-13.0508216223155));
#5793=CARTESIAN_POINT('Ctrl Pts',(48.706329375,34.687500006828,1.293339198242E-14));
#5794=CARTESIAN_POINT('Ctrl Pts',(48.706329375,34.4791666734946,13.0508216223155));
#5795=CARTESIAN_POINT('Ctrl Pts',(42.1809185638422,34.2708333401613,24.3531646875));
#5796=CARTESIAN_POINT('Ctrl Pts',(35.6555077526845,34.062500006828,35.6555077526845));
#5797=CARTESIAN_POINT('Ctrl Pts',(24.3531646875,33.8541666734946,42.1809185638422));
#5798=CARTESIAN_POINT('Ctrl Pts',(13.0508216223155,33.6458333401613,48.706329375));
#5799=CARTESIAN_POINT('Ctrl Pts',(-9.95098946405443E-15,33.437500006828,
48.706329375));
#5800=CARTESIAN_POINT('Ctrl Pts',(-13.0508216223155,33.2291666734946,48.706329375));
#5801=CARTESIAN_POINT('Ctrl Pts',(-24.3531646875,33.0208333401613,42.1809185638423));
#5802=CARTESIAN_POINT('Ctrl Pts',(-35.6555077526845,32.812500006828,35.6555077526845));
#5803=CARTESIAN_POINT('Ctrl Pts',(-42.1809185638422,32.6041666734946,24.3531646875));
#5804=CARTESIAN_POINT('Ctrl Pts',(-48.706329375,32.3958333401613,13.0508216223155));
#5805=CARTESIAN_POINT('Ctrl Pts',(-48.706329375,32.187500006828,-1.8898197019151E-14));
#5806=CARTESIAN_POINT('Ctrl Pts',(-48.706329375,31.9791666734946,-13.0508216223155));
#5807=CARTESIAN_POINT('Ctrl Pts',(-42.1809185638422,31.7708333401613,-24.3531646875));
#5808=CARTESIAN_POINT('Ctrl Pts',(-35.6555077526845,31.562500006828,-35.6555077526845));
#5809=CARTESIAN_POINT('Ctrl Pts',(-24.3531646875,31.3541666734946,-42.1809185638423));
#5810=CARTESIAN_POINT('Ctrl Pts',(-13.0508216223155,31.1458333401613,-48.706329375));
#5811=CARTESIAN_POINT('Ctrl Pts',(1.59157945007855E-14,30.937500006828,
-48.706329375));
#5812=CARTESIAN_POINT('Ctrl Pts',(13.0508216223155,30.7291666734946,-48.706329375));
#5813=CARTESIAN_POINT('Ctrl Pts',(24.3531646875,30.5208333401613,-42.1809185638422));
#5814=CARTESIAN_POINT('Ctrl Pts',(35.6555077526845,30.312500006828,-35.6555077526845));
#5815=CARTESIAN_POINT('Ctrl Pts',(42.1809185638422,30.1041666734946,-24.3531646875));
#5816=CARTESIAN_POINT('Ctrl Pts',(48.706329375,29.8958333401613,-13.0508216223155));
#5817=CARTESIAN_POINT('Ctrl Pts',(48.706329375,29.687500006828,1.293339198242E-14));
#5818=CARTESIAN_POINT('Ctrl Pts',(48.706329375,29.4791666734946,13.0508216223155));
#5819=CARTESIAN_POINT('Ctrl Pts',(42.1809185638422,29.2708333401613,24.3531646875));
#5820=CARTESIAN_POINT('Ctrl Pts',(35.6555077526845,29.062500006828,35.6555077526845));
#5821=CARTESIAN_POINT('Ctrl Pts',(24.3531646875,28.8541666734946,42.1809185638422));
#5822=CARTESIAN_POINT('Ctrl Pts',(13.0508216223155,28.6458333401613,48.706329375));
#5823=CARTESIAN_POINT('Ctrl Pts',(-9.95098946405443E-15,28.437500006828,
48.706329375));
#5824=CARTESIAN_POINT('Ctrl Pts',(-13.0508216223155,28.2291666734946,48.706329375));
#5825=CARTESIAN_POINT('Ctrl Pts',(-24.3531646875,28.0208333401613,42.1809185638423));
#5826=CARTESIAN_POINT('Ctrl Pts',(-35.6555077526845,27.812500006828,35.6555077526845));
#5827=CARTESIAN_POINT('Ctrl Pts',(-42.1809185638422,27.6041666734946,24.3531646875));
#5828=CARTESIAN_POINT('Ctrl Pts',(-48.706329375,27.3958333401613,13.0508216223155));
#5829=CARTESIAN_POINT('Ctrl Pts',(-48.706329375,27.187500006828,-1.8898197019151E-14));
#5830=CARTESIAN_POINT('',(3.61292728433799,55.8792520480092,-48.5721450795008));
#5831=CARTESIAN_POINT('',(48.5134353784345,54.7574536451604,-4.33048599679674));
#5832=CARTESIAN_POINT('Ctrl Pts',(3.61292728433799,55.8792520480093,-48.5721450795008));
#5833=CARTESIAN_POINT('Ctrl Pts',(14.7133549689477,55.6985216017707,-47.7464652997852));
#5834=CARTESIAN_POINT('Ctrl Pts',(24.3531646875,55.5208333401613,-42.1809185638422));
#5835=CARTESIAN_POINT('Ctrl Pts',(35.6555077526845,55.312500006828,-35.6555077526845));
#5836=CARTESIAN_POINT('Ctrl Pts',(42.1809185638422,55.1041666734946,-24.3531646875));
#5837=CARTESIAN_POINT('Ctrl Pts',(47.5573898704235,54.9325149229327,-15.0408432190651));
#5838=CARTESIAN_POINT('Ctrl Pts',(48.5134353784344,54.7574536451604,-4.33048599679674));
#5839=CARTESIAN_POINT('Origin',(-4513.80899778907,8008.28355048454,-4.33048540714616));
#5840=CARTESIAN_POINT('Ctrl Pts',(3.61292728433799,54.3132892765089,-45.8578974271399));
#5841=CARTESIAN_POINT('Ctrl Pts',(3.612927284338,54.4468822859549,-46.089460636719));
#5842=CARTESIAN_POINT('Ctrl Pts',(3.61292728433798,54.7140705280012,-46.5525857733052));
#5843=CARTESIAN_POINT('Ctrl Pts',(3.61292728433799,54.9812630238615,-47.0157084557285));
#5844=CARTESIAN_POINT('Ctrl Pts',(3.61292728433799,55.3696539378594,-47.6888965792834));
#5845=CARTESIAN_POINT('Ctrl Pts',(3.61292728433799,55.624451287085,-48.1305218136162));
#5846=CARTESIAN_POINT('Ctrl Pts',(3.61292728433799,55.8792520480092,-48.5721450795008));
#5847=CARTESIAN_POINT('Ctrl Pts',(-46.,55.6250000136559,0.));
#5848=CARTESIAN_POINT('Ctrl Pts',(-46.,55.4166666803226,-12.3256628518316));
#5849=CARTESIAN_POINT('Ctrl Pts',(-39.8371685740842,55.2083333469893,-23.));
#5850=CARTESIAN_POINT('Ctrl Pts',(-33.6743371481684,55.0000000136559,-33.6743371481684));
#5851=CARTESIAN_POINT('Ctrl Pts',(-23.,54.7916666803226,-39.8371685740842));
#5852=CARTESIAN_POINT('Ctrl Pts',(-12.3256628518317,54.5833333469893,-46.));
#5853=CARTESIAN_POINT('Ctrl Pts',(-2.81668763803891E-15,54.3750000136559,
-46.));
#5854=CARTESIAN_POINT('Ctrl Pts',(12.3256628518316,54.1666666803226,-46.));
#5855=CARTESIAN_POINT('Ctrl Pts',(23.,53.9583333469893,-39.8371685740842));
#5856=CARTESIAN_POINT('Ctrl Pts',(33.6743371481683,53.7500000136559,-33.6743371481684));
#5857=CARTESIAN_POINT('Ctrl Pts',(39.8371685740842,53.5416666803226,-23.));
#5858=CARTESIAN_POINT('Ctrl Pts',(46.,53.3333333469893,-12.3256628518317));
#5859=CARTESIAN_POINT('Ctrl Pts',(46.,53.1250000136559,-5.63337527607782E-15));
#5860=CARTESIAN_POINT('Ctrl Pts',(46.,52.9166666803226,12.3256628518316));
#5861=CARTESIAN_POINT('Ctrl Pts',(39.8371685740842,52.7083333469893,23.));
#5862=CARTESIAN_POINT('Ctrl Pts',(33.6743371481684,52.5000000136559,33.6743371481683));
#5863=CARTESIAN_POINT('Ctrl Pts',(23.,52.2916666803226,39.8371685740842));
#5864=CARTESIAN_POINT('Ctrl Pts',(12.3256628518317,52.0833333469893,46.));
#5865=CARTESIAN_POINT('Ctrl Pts',(8.45006291411674E-15,51.8750000136559,
46.));
#5866=CARTESIAN_POINT('Ctrl Pts',(-12.3256628518316,51.6666666803226,46.));
#5867=CARTESIAN_POINT('Ctrl Pts',(-23.,51.4583333469893,39.8371685740842));
#5868=CARTESIAN_POINT('Ctrl Pts',(-33.6743371481683,51.2500000136559,33.6743371481684));
#5869=CARTESIAN_POINT('Ctrl Pts',(-39.8371685740842,51.0416666803226,23.));
#5870=CARTESIAN_POINT('Ctrl Pts',(-46.,50.8333333469893,12.3256628518317));
#5871=CARTESIAN_POINT('Ctrl Pts',(-46.,50.6250000136559,0.));
#5872=CARTESIAN_POINT('Ctrl Pts',(-46.,50.4166666803226,-12.3256628518316));
#5873=CARTESIAN_POINT('Ctrl Pts',(-39.8371685740842,50.2083333469893,-23.));
#5874=CARTESIAN_POINT('Ctrl Pts',(-33.6743371481684,50.0000000136559,-33.6743371481684));
#5875=CARTESIAN_POINT('Ctrl Pts',(-23.,49.7916666803226,-39.8371685740842));
#5876=CARTESIAN_POINT('Ctrl Pts',(-12.3256628518317,49.5833333469893,-46.));
#5877=CARTESIAN_POINT('Ctrl Pts',(-2.81668763803891E-15,49.3750000136559,
-46.));
#5878=CARTESIAN_POINT('Ctrl Pts',(12.3256628518316,49.1666666803226,-46.));
#5879=CARTESIAN_POINT('Ctrl Pts',(23.,48.9583333469893,-39.8371685740842));
#5880=CARTESIAN_POINT('Ctrl Pts',(33.6743371481683,48.7500000136559,-33.6743371481684));
#5881=CARTESIAN_POINT('Ctrl Pts',(39.8371685740842,48.5416666803226,-23.));
#5882=CARTESIAN_POINT('Ctrl Pts',(46.,48.3333333469893,-12.3256628518317));
#5883=CARTESIAN_POINT('Ctrl Pts',(46.,48.1250000136559,-5.63337527607782E-15));
#5884=CARTESIAN_POINT('Ctrl Pts',(46.,47.9166666803226,12.3256628518316));
#5885=CARTESIAN_POINT('Ctrl Pts',(39.8371685740842,47.7083333469893,23.));
#5886=CARTESIAN_POINT('Ctrl Pts',(33.6743371481684,47.5000000136559,33.6743371481683));
#5887=CARTESIAN_POINT('Ctrl Pts',(23.,47.2916666803226,39.8371685740842));
#5888=CARTESIAN_POINT('Ctrl Pts',(12.3256628518317,47.0833333469893,46.));
#5889=CARTESIAN_POINT('Ctrl Pts',(8.45006291411674E-15,46.8750000136559,
46.));
#5890=CARTESIAN_POINT('Ctrl Pts',(-12.3256628518316,46.6666666803226,46.));
#5891=CARTESIAN_POINT('Ctrl Pts',(-23.,46.4583333469893,39.8371685740842));
#5892=CARTESIAN_POINT('Ctrl Pts',(-33.6743371481683,46.2500000136559,33.6743371481684));
#5893=CARTESIAN_POINT('Ctrl Pts',(-39.8371685740842,46.0416666803226,23.));
#5894=CARTESIAN_POINT('Ctrl Pts',(-46.,45.8333333469892,12.3256628518317));
#5895=CARTESIAN_POINT('Ctrl Pts',(-46.,45.6250000136559,0.));
#5896=CARTESIAN_POINT('Ctrl Pts',(-46.,45.4166666803226,-12.3256628518316));
#5897=CARTESIAN_POINT('Ctrl Pts',(-39.8371685740842,45.2083333469893,-23.));
#5898=CARTESIAN_POINT('Ctrl Pts',(-33.6743371481684,45.0000000136559,-33.6743371481684));
#5899=CARTESIAN_POINT('Ctrl Pts',(-23.,44.7916666803226,-39.8371685740842));
#5900=CARTESIAN_POINT('Ctrl Pts',(-12.3256628518317,44.5833333469893,-46.));
#5901=CARTESIAN_POINT('Ctrl Pts',(-2.81668763803891E-15,44.3750000136559,
-46.));
#5902=CARTESIAN_POINT('Ctrl Pts',(12.3256628518316,44.1666666803226,-46.));
#5903=CARTESIAN_POINT('Ctrl Pts',(23.,43.9583333469893,-39.8371685740842));
#5904=CARTESIAN_POINT('Ctrl Pts',(33.6743371481683,43.7500000136559,-33.6743371481684));
#5905=CARTESIAN_POINT('Ctrl Pts',(39.8371685740842,43.5416666803226,-23.));
#5906=CARTESIAN_POINT('Ctrl Pts',(46.,43.3333333469893,-12.3256628518317));
#5907=CARTESIAN_POINT('Ctrl Pts',(46.,43.1250000136559,-5.63337527607782E-15));
#5908=CARTESIAN_POINT('Ctrl Pts',(46.,42.9166666803226,12.3256628518316));
#5909=CARTESIAN_POINT('Ctrl Pts',(39.8371685740842,42.7083333469893,23.));
#5910=CARTESIAN_POINT('Ctrl Pts',(33.6743371481684,42.5000000136559,33.6743371481683));
#5911=CARTESIAN_POINT('Ctrl Pts',(23.,42.2916666803226,39.8371685740842));
#5912=CARTESIAN_POINT('Ctrl Pts',(12.3256628518317,42.0833333469893,46.));
#5913=CARTESIAN_POINT('Ctrl Pts',(8.45006291411674E-15,41.8750000136559,
46.));
#5914=CARTESIAN_POINT('Ctrl Pts',(-12.3256628518316,41.6666666803226,46.));
#5915=CARTESIAN_POINT('Ctrl Pts',(-23.,41.4583333469893,39.8371685740842));
#5916=CARTESIAN_POINT('Ctrl Pts',(-33.6743371481683,41.2500000136559,33.6743371481684));
#5917=CARTESIAN_POINT('Ctrl Pts',(-39.8371685740842,41.0416666803226,23.));
#5918=CARTESIAN_POINT('Ctrl Pts',(-46.,40.8333333469893,12.3256628518317));
#5919=CARTESIAN_POINT('Ctrl Pts',(-46.,40.6250000136559,0.));
#5920=CARTESIAN_POINT('Ctrl Pts',(-46.,40.4166666803226,-12.3256628518316));
#5921=CARTESIAN_POINT('Ctrl Pts',(-39.8371685740842,40.2083333469893,-23.));
#5922=CARTESIAN_POINT('Ctrl Pts',(-33.6743371481684,40.0000000136559,-33.6743371481684));
#5923=CARTESIAN_POINT('Ctrl Pts',(-23.,39.7916666803226,-39.8371685740842));
#5924=CARTESIAN_POINT('Ctrl Pts',(-12.3256628518317,39.5833333469893,-46.));
#5925=CARTESIAN_POINT('Ctrl Pts',(-2.81668763803891E-15,39.3750000136559,
-46.));
#5926=CARTESIAN_POINT('Ctrl Pts',(12.3256628518316,39.1666666803226,-46.));
#5927=CARTESIAN_POINT('Ctrl Pts',(23.,38.9583333469893,-39.8371685740842));
#5928=CARTESIAN_POINT('Ctrl Pts',(33.6743371481683,38.7500000136559,-33.6743371481684));
#5929=CARTESIAN_POINT('Ctrl Pts',(39.8371685740842,38.5416666803226,-23.));
#5930=CARTESIAN_POINT('Ctrl Pts',(46.,38.3333333469893,-12.3256628518317));
#5931=CARTESIAN_POINT('Ctrl Pts',(46.,38.1250000136559,-5.63337527607782E-15));
#5932=CARTESIAN_POINT('Ctrl Pts',(46.,37.9166666803226,12.3256628518316));
#5933=CARTESIAN_POINT('Ctrl Pts',(39.8371685740842,37.7083333469893,23.));
#5934=CARTESIAN_POINT('Ctrl Pts',(33.6743371481684,37.5000000136559,33.6743371481683));
#5935=CARTESIAN_POINT('Ctrl Pts',(23.,37.2916666803226,39.8371685740842));
#5936=CARTESIAN_POINT('Ctrl Pts',(12.3256628518317,37.0833333469893,46.));
#5937=CARTESIAN_POINT('Ctrl Pts',(8.45006291411674E-15,36.8750000136559,
46.));
#5938=CARTESIAN_POINT('Ctrl Pts',(-12.3256628518316,36.6666666803226,46.));
#5939=CARTESIAN_POINT('Ctrl Pts',(-23.,36.4583333469893,39.8371685740842));
#5940=CARTESIAN_POINT('Ctrl Pts',(-33.6743371481683,36.2500000136559,33.6743371481684));
#5941=CARTESIAN_POINT('Ctrl Pts',(-39.8371685740842,36.0416666803226,23.));
#5942=CARTESIAN_POINT('Ctrl Pts',(-46.,35.8333333469893,12.3256628518317));
#5943=CARTESIAN_POINT('Ctrl Pts',(-46.,35.6250000136559,0.));
#5944=CARTESIAN_POINT('Ctrl Pts',(-46.,35.4166666803226,-12.3256628518316));
#5945=CARTESIAN_POINT('Ctrl Pts',(-39.8371685740842,35.2083333469893,-23.));
#5946=CARTESIAN_POINT('Ctrl Pts',(-33.6743371481684,35.0000000136559,-33.6743371481684));
#5947=CARTESIAN_POINT('Ctrl Pts',(-23.,34.7916666803226,-39.8371685740842));
#5948=CARTESIAN_POINT('Ctrl Pts',(-12.3256628518317,34.5833333469893,-46.));
#5949=CARTESIAN_POINT('Ctrl Pts',(-2.81668763803891E-15,34.3750000136559,
-46.));
#5950=CARTESIAN_POINT('Ctrl Pts',(12.3256628518316,34.1666666803226,-46.));
#5951=CARTESIAN_POINT('Ctrl Pts',(23.,33.9583333469893,-39.8371685740842));
#5952=CARTESIAN_POINT('Ctrl Pts',(33.6743371481683,33.7500000136559,-33.6743371481684));
#5953=CARTESIAN_POINT('Ctrl Pts',(39.8371685740842,33.5416666803226,-23.));
#5954=CARTESIAN_POINT('Ctrl Pts',(46.,33.3333333469893,-12.3256628518317));
#5955=CARTESIAN_POINT('Ctrl Pts',(46.,33.1250000136559,-5.63337527607782E-15));
#5956=CARTESIAN_POINT('Ctrl Pts',(46.,32.9166666803226,12.3256628518316));
#5957=CARTESIAN_POINT('Ctrl Pts',(39.8371685740842,32.7083333469893,23.));
#5958=CARTESIAN_POINT('Ctrl Pts',(33.6743371481684,32.5000000136559,33.6743371481683));
#5959=CARTESIAN_POINT('Ctrl Pts',(23.,32.2916666803226,39.8371685740842));
#5960=CARTESIAN_POINT('Ctrl Pts',(12.3256628518317,32.0833333469893,46.));
#5961=CARTESIAN_POINT('Ctrl Pts',(8.45006291411674E-15,31.8750000136559,
46.));
#5962=CARTESIAN_POINT('Ctrl Pts',(-12.3256628518316,31.6666666803226,46.));
#5963=CARTESIAN_POINT('Ctrl Pts',(-23.,31.4583333469893,39.8371685740842));
#5964=CARTESIAN_POINT('Ctrl Pts',(-33.6743371481683,31.2500000136559,33.6743371481684));
#5965=CARTESIAN_POINT('Ctrl Pts',(-39.8371685740842,31.0416666803226,23.));
#5966=CARTESIAN_POINT('Ctrl Pts',(-46.,30.8333333469893,12.3256628518317));
#5967=CARTESIAN_POINT('Ctrl Pts',(-46.,30.6250000136559,0.));
#5968=CARTESIAN_POINT('Ctrl Pts',(-46.,30.4166666803226,-12.3256628518316));
#5969=CARTESIAN_POINT('Ctrl Pts',(-39.8371685740842,30.2083333469893,-23.));
#5970=CARTESIAN_POINT('Ctrl Pts',(-33.6743371481684,30.0000000136559,-33.6743371481684));
#5971=CARTESIAN_POINT('Ctrl Pts',(-23.,29.7916666803226,-39.8371685740842));
#5972=CARTESIAN_POINT('Ctrl Pts',(-12.3256628518317,29.5833333469893,-46.));
#5973=CARTESIAN_POINT('Ctrl Pts',(-2.81668763803891E-15,29.3750000136559,
-46.));
#5974=CARTESIAN_POINT('Ctrl Pts',(12.3256628518316,29.1666666803226,-46.));
#5975=CARTESIAN_POINT('Ctrl Pts',(23.,28.9583333469893,-39.8371685740842));
#5976=CARTESIAN_POINT('Ctrl Pts',(33.6743371481683,28.7500000136559,-33.6743371481684));
#5977=CARTESIAN_POINT('Ctrl Pts',(39.8371685740842,28.5416666803226,-23.));
#5978=CARTESIAN_POINT('Ctrl Pts',(46.,28.3333333469893,-12.3256628518317));
#5979=CARTESIAN_POINT('Ctrl Pts',(46.,28.1250000136559,-5.63337527607782E-15));
#5980=CARTESIAN_POINT('Ctrl Pts',(46.,27.9166666803226,12.3256628518316));
#5981=CARTESIAN_POINT('Ctrl Pts',(39.8371685740842,27.7083333469893,23.));
#5982=CARTESIAN_POINT('Ctrl Pts',(33.6743371481684,27.5000000136559,33.6743371481683));
#5983=CARTESIAN_POINT('Ctrl Pts',(23.,27.2916666803226,39.8371685740842));
#5984=CARTESIAN_POINT('Ctrl Pts',(12.3256628518317,27.0833333469893,46.));
#5985=CARTESIAN_POINT('Ctrl Pts',(8.45006291411674E-15,26.8750000136559,
46.));
#5986=CARTESIAN_POINT('Ctrl Pts',(-12.3256628518316,26.6666666803226,46.));
#5987=CARTESIAN_POINT('Ctrl Pts',(-23.,26.4583333469893,39.8371685740842));
#5988=CARTESIAN_POINT('Ctrl Pts',(-33.6743371481683,26.2500000136559,33.6743371481684));
#5989=CARTESIAN_POINT('Ctrl Pts',(-39.8371685740842,26.0416666803226,23.));
#5990=CARTESIAN_POINT('Ctrl Pts',(-46.,25.8333333469893,12.3256628518317));
#5991=CARTESIAN_POINT('Ctrl Pts',(-46.,25.6250000136559,0.));
#5992=CARTESIAN_POINT('Ctrl Pts',(-48.706329375,57.187500006828,-1.8898197019151E-14));
#5993=CARTESIAN_POINT('Ctrl Pts',(-48.706329375,56.9791666734946,-13.0508216223155));
#5994=CARTESIAN_POINT('Ctrl Pts',(-42.1809185638422,56.7708333401613,-24.3531646875));
#5995=CARTESIAN_POINT('Ctrl Pts',(-35.6555077526845,56.562500006828,-35.6555077526845));
#5996=CARTESIAN_POINT('Ctrl Pts',(-24.3531646875,56.3541666734946,-42.1809185638423));
#5997=CARTESIAN_POINT('Ctrl Pts',(-13.0508216223155,56.1458333401613,-48.706329375));
#5998=CARTESIAN_POINT('Ctrl Pts',(1.59157945007855E-14,55.937500006828,
-48.706329375));
#5999=CARTESIAN_POINT('Ctrl Pts',(13.0508216223155,55.7291666734946,-48.706329375));
#6000=CARTESIAN_POINT('Ctrl Pts',(24.3531646875,55.5208333401613,-42.1809185638422));
#6001=CARTESIAN_POINT('Ctrl Pts',(35.6555077526845,55.312500006828,-35.6555077526845));
#6002=CARTESIAN_POINT('Ctrl Pts',(42.1809185638422,55.1041666734946,-24.3531646875));
#6003=CARTESIAN_POINT('Ctrl Pts',(48.706329375,54.8958333401613,-13.0508216223155));
#6004=CARTESIAN_POINT('Ctrl Pts',(48.706329375,54.687500006828,1.293339198242E-14));
#6005=CARTESIAN_POINT('Ctrl Pts',(48.706329375,54.4791666734946,13.0508216223155));
#6006=CARTESIAN_POINT('Ctrl Pts',(42.1809185638422,54.2708333401613,24.3531646875));
#6007=CARTESIAN_POINT('Ctrl Pts',(35.6555077526845,54.062500006828,35.6555077526845));
#6008=CARTESIAN_POINT('Ctrl Pts',(24.3531646875,53.8541666734946,42.1809185638422));
#6009=CARTESIAN_POINT('Ctrl Pts',(13.0508216223155,53.6458333401613,48.706329375));
#6010=CARTESIAN_POINT('Ctrl Pts',(-9.95098946405443E-15,53.437500006828,
48.706329375));
#6011=CARTESIAN_POINT('Ctrl Pts',(-13.0508216223155,53.2291666734946,48.706329375));
#6012=CARTESIAN_POINT('Ctrl Pts',(-24.3531646875,53.0208333401613,42.1809185638423));
#6013=CARTESIAN_POINT('Ctrl Pts',(-35.6555077526845,52.812500006828,35.6555077526845));
#6014=CARTESIAN_POINT('Ctrl Pts',(-42.1809185638422,52.6041666734946,24.3531646875));
#6015=CARTESIAN_POINT('Ctrl Pts',(-48.706329375,52.3958333401613,13.0508216223155));
#6016=CARTESIAN_POINT('Ctrl Pts',(-48.706329375,52.187500006828,-1.8898197019151E-14));
#6017=CARTESIAN_POINT('Ctrl Pts',(-48.706329375,51.9791666734946,-13.0508216223155));
#6018=CARTESIAN_POINT('Ctrl Pts',(-42.1809185638422,51.7708333401613,-24.3531646875));
#6019=CARTESIAN_POINT('Ctrl Pts',(-35.6555077526845,51.562500006828,-35.6555077526845));
#6020=CARTESIAN_POINT('Ctrl Pts',(-24.3531646875,51.3541666734946,-42.1809185638423));
#6021=CARTESIAN_POINT('Ctrl Pts',(-13.0508216223155,51.1458333401613,-48.706329375));
#6022=CARTESIAN_POINT('Ctrl Pts',(1.59157945007855E-14,50.937500006828,
-48.706329375));
#6023=CARTESIAN_POINT('Ctrl Pts',(13.0508216223155,50.7291666734946,-48.706329375));
#6024=CARTESIAN_POINT('Ctrl Pts',(24.3531646875,50.5208333401613,-42.1809185638422));
#6025=CARTESIAN_POINT('Ctrl Pts',(35.6555077526845,50.312500006828,-35.6555077526845));
#6026=CARTESIAN_POINT('Ctrl Pts',(42.1809185638422,50.1041666734946,-24.3531646875));
#6027=CARTESIAN_POINT('Ctrl Pts',(48.706329375,49.8958333401613,-13.0508216223155));
#6028=CARTESIAN_POINT('Ctrl Pts',(48.706329375,49.687500006828,1.293339198242E-14));
#6029=CARTESIAN_POINT('Ctrl Pts',(48.706329375,49.4791666734946,13.0508216223155));
#6030=CARTESIAN_POINT('Ctrl Pts',(42.1809185638422,49.2708333401613,24.3531646875));
#6031=CARTESIAN_POINT('Ctrl Pts',(35.6555077526845,49.062500006828,35.6555077526845));
#6032=CARTESIAN_POINT('Ctrl Pts',(24.3531646875,48.8541666734946,42.1809185638422));
#6033=CARTESIAN_POINT('Ctrl Pts',(13.0508216223155,48.6458333401613,48.706329375));
#6034=CARTESIAN_POINT('Ctrl Pts',(-9.95098946405443E-15,48.437500006828,
48.706329375));
#6035=CARTESIAN_POINT('Ctrl Pts',(-13.0508216223155,48.2291666734946,48.706329375));
#6036=CARTESIAN_POINT('Ctrl Pts',(-24.3531646875,48.0208333401613,42.1809185638423));
#6037=CARTESIAN_POINT('Ctrl Pts',(-35.6555077526845,47.812500006828,35.6555077526845));
#6038=CARTESIAN_POINT('Ctrl Pts',(-42.1809185638422,47.6041666734946,24.3531646875));
#6039=CARTESIAN_POINT('Ctrl Pts',(-48.706329375,47.3958333401613,13.0508216223155));
#6040=CARTESIAN_POINT('Ctrl Pts',(-48.706329375,47.187500006828,-1.8898197019151E-14));
#6041=CARTESIAN_POINT('Ctrl Pts',(-48.706329375,46.9791666734946,-13.0508216223155));
#6042=CARTESIAN_POINT('Ctrl Pts',(-42.1809185638422,46.7708333401613,-24.3531646875));
#6043=CARTESIAN_POINT('Ctrl Pts',(-35.6555077526845,46.562500006828,-35.6555077526845));
#6044=CARTESIAN_POINT('Ctrl Pts',(-24.3531646875,46.3541666734946,-42.1809185638423));
#6045=CARTESIAN_POINT('Ctrl Pts',(-13.0508216223155,46.1458333401613,-48.706329375));
#6046=CARTESIAN_POINT('Ctrl Pts',(1.59157945007855E-14,45.937500006828,
-48.706329375));
#6047=CARTESIAN_POINT('Ctrl Pts',(13.0508216223155,45.7291666734946,-48.706329375));
#6048=CARTESIAN_POINT('Ctrl Pts',(24.3531646875,45.5208333401613,-42.1809185638422));
#6049=CARTESIAN_POINT('Ctrl Pts',(35.6555077526845,45.312500006828,-35.6555077526845));
#6050=CARTESIAN_POINT('Ctrl Pts',(42.1809185638422,45.1041666734946,-24.3531646875));
#6051=CARTESIAN_POINT('Ctrl Pts',(48.706329375,44.8958333401613,-13.0508216223155));
#6052=CARTESIAN_POINT('Ctrl Pts',(48.706329375,44.687500006828,1.293339198242E-14));
#6053=CARTESIAN_POINT('Ctrl Pts',(48.706329375,44.4791666734946,13.0508216223155));
#6054=CARTESIAN_POINT('Ctrl Pts',(42.1809185638422,44.2708333401613,24.3531646875));
#6055=CARTESIAN_POINT('Ctrl Pts',(35.6555077526845,44.062500006828,35.6555077526845));
#6056=CARTESIAN_POINT('Ctrl Pts',(24.3531646875,43.8541666734946,42.1809185638422));
#6057=CARTESIAN_POINT('Ctrl Pts',(13.0508216223155,43.6458333401613,48.706329375));
#6058=CARTESIAN_POINT('Ctrl Pts',(-9.95098946405443E-15,43.437500006828,
48.706329375));
#6059=CARTESIAN_POINT('Ctrl Pts',(-13.0508216223155,43.2291666734946,48.706329375));
#6060=CARTESIAN_POINT('Ctrl Pts',(-24.3531646875,43.0208333401613,42.1809185638423));
#6061=CARTESIAN_POINT('Ctrl Pts',(-35.6555077526845,42.812500006828,35.6555077526845));
#6062=CARTESIAN_POINT('Ctrl Pts',(-42.1809185638422,42.6041666734946,24.3531646875));
#6063=CARTESIAN_POINT('Ctrl Pts',(-48.706329375,42.3958333401613,13.0508216223155));
#6064=CARTESIAN_POINT('Ctrl Pts',(-48.706329375,42.187500006828,-1.8898197019151E-14));
#6065=CARTESIAN_POINT('Ctrl Pts',(-48.706329375,41.9791666734946,-13.0508216223155));
#6066=CARTESIAN_POINT('Ctrl Pts',(-42.1809185638422,41.7708333401613,-24.3531646875));
#6067=CARTESIAN_POINT('Ctrl Pts',(-35.6555077526845,41.562500006828,-35.6555077526845));
#6068=CARTESIAN_POINT('Ctrl Pts',(-24.3531646875,41.3541666734946,-42.1809185638423));
#6069=CARTESIAN_POINT('Ctrl Pts',(-13.0508216223155,41.1458333401613,-48.706329375));
#6070=CARTESIAN_POINT('Ctrl Pts',(1.59157945007855E-14,40.937500006828,
-48.706329375));
#6071=CARTESIAN_POINT('Ctrl Pts',(13.0508216223155,40.7291666734946,-48.706329375));
#6072=CARTESIAN_POINT('Ctrl Pts',(24.3531646875,40.5208333401613,-42.1809185638422));
#6073=CARTESIAN_POINT('Ctrl Pts',(35.6555077526845,40.312500006828,-35.6555077526845));
#6074=CARTESIAN_POINT('Ctrl Pts',(42.1809185638422,40.1041666734946,-24.3531646875));
#6075=CARTESIAN_POINT('Ctrl Pts',(48.706329375,39.8958333401613,-13.0508216223155));
#6076=CARTESIAN_POINT('Ctrl Pts',(48.706329375,39.687500006828,1.293339198242E-14));
#6077=CARTESIAN_POINT('Ctrl Pts',(48.706329375,39.4791666734946,13.0508216223155));
#6078=CARTESIAN_POINT('Ctrl Pts',(42.1809185638422,39.2708333401613,24.3531646875));
#6079=CARTESIAN_POINT('Ctrl Pts',(35.6555077526845,39.062500006828,35.6555077526845));
#6080=CARTESIAN_POINT('Ctrl Pts',(24.3531646875,38.8541666734946,42.1809185638422));
#6081=CARTESIAN_POINT('Ctrl Pts',(13.0508216223155,38.6458333401613,48.706329375));
#6082=CARTESIAN_POINT('Ctrl Pts',(-9.95098946405443E-15,38.437500006828,
48.706329375));
#6083=CARTESIAN_POINT('Ctrl Pts',(-13.0508216223155,38.2291666734946,48.706329375));
#6084=CARTESIAN_POINT('Ctrl Pts',(-24.3531646875,38.0208333401613,42.1809185638423));
#6085=CARTESIAN_POINT('Ctrl Pts',(-35.6555077526845,37.812500006828,35.6555077526845));
#6086=CARTESIAN_POINT('Ctrl Pts',(-42.1809185638422,37.6041666734946,24.3531646875));
#6087=CARTESIAN_POINT('Ctrl Pts',(-48.706329375,37.3958333401613,13.0508216223155));
#6088=CARTESIAN_POINT('Ctrl Pts',(-48.706329375,37.187500006828,-1.8898197019151E-14));
#6089=CARTESIAN_POINT('Ctrl Pts',(-48.706329375,36.9791666734946,-13.0508216223155));
#6090=CARTESIAN_POINT('Ctrl Pts',(-42.1809185638422,36.7708333401613,-24.3531646875));
#6091=CARTESIAN_POINT('Ctrl Pts',(-35.6555077526845,36.562500006828,-35.6555077526845));
#6092=CARTESIAN_POINT('Ctrl Pts',(-24.3531646875,36.3541666734946,-42.1809185638423));
#6093=CARTESIAN_POINT('Ctrl Pts',(-13.0508216223155,36.1458333401613,-48.706329375));
#6094=CARTESIAN_POINT('Ctrl Pts',(1.59157945007855E-14,35.937500006828,
-48.706329375));
#6095=CARTESIAN_POINT('Ctrl Pts',(13.0508216223155,35.7291666734946,-48.706329375));
#6096=CARTESIAN_POINT('Ctrl Pts',(24.3531646875,35.5208333401613,-42.1809185638422));
#6097=CARTESIAN_POINT('Ctrl Pts',(35.6555077526845,35.312500006828,-35.6555077526845));
#6098=CARTESIAN_POINT('Ctrl Pts',(42.1809185638422,35.1041666734946,-24.3531646875));
#6099=CARTESIAN_POINT('Ctrl Pts',(48.706329375,34.8958333401613,-13.0508216223155));
#6100=CARTESIAN_POINT('Ctrl Pts',(48.706329375,34.687500006828,1.293339198242E-14));
#6101=CARTESIAN_POINT('Ctrl Pts',(48.706329375,34.4791666734946,13.0508216223155));
#6102=CARTESIAN_POINT('Ctrl Pts',(42.1809185638422,34.2708333401613,24.3531646875));
#6103=CARTESIAN_POINT('Ctrl Pts',(35.6555077526845,34.062500006828,35.6555077526845));
#6104=CARTESIAN_POINT('Ctrl Pts',(24.3531646875,33.8541666734946,42.1809185638422));
#6105=CARTESIAN_POINT('Ctrl Pts',(13.0508216223155,33.6458333401613,48.706329375));
#6106=CARTESIAN_POINT('Ctrl Pts',(-9.95098946405443E-15,33.437500006828,
48.706329375));
#6107=CARTESIAN_POINT('Ctrl Pts',(-13.0508216223155,33.2291666734946,48.706329375));
#6108=CARTESIAN_POINT('Ctrl Pts',(-24.3531646875,33.0208333401613,42.1809185638423));
#6109=CARTESIAN_POINT('Ctrl Pts',(-35.6555077526845,32.812500006828,35.6555077526845));
#6110=CARTESIAN_POINT('Ctrl Pts',(-42.1809185638422,32.6041666734946,24.3531646875));
#6111=CARTESIAN_POINT('Ctrl Pts',(-48.706329375,32.3958333401613,13.0508216223155));
#6112=CARTESIAN_POINT('Ctrl Pts',(-48.706329375,32.187500006828,-1.8898197019151E-14));
#6113=CARTESIAN_POINT('Ctrl Pts',(-48.706329375,31.9791666734946,-13.0508216223155));
#6114=CARTESIAN_POINT('Ctrl Pts',(-42.1809185638422,31.7708333401613,-24.3531646875));
#6115=CARTESIAN_POINT('Ctrl Pts',(-35.6555077526845,31.562500006828,-35.6555077526845));
#6116=CARTESIAN_POINT('Ctrl Pts',(-24.3531646875,31.3541666734946,-42.1809185638423));
#6117=CARTESIAN_POINT('Ctrl Pts',(-13.0508216223155,31.1458333401613,-48.706329375));
#6118=CARTESIAN_POINT('Ctrl Pts',(1.59157945007855E-14,30.937500006828,
-48.706329375));
#6119=CARTESIAN_POINT('Ctrl Pts',(13.0508216223155,30.7291666734946,-48.706329375));
#6120=CARTESIAN_POINT('Ctrl Pts',(24.3531646875,30.5208333401613,-42.1809185638422));
#6121=CARTESIAN_POINT('Ctrl Pts',(35.6555077526845,30.312500006828,-35.6555077526845));
#6122=CARTESIAN_POINT('Ctrl Pts',(42.1809185638422,30.1041666734946,-24.3531646875));
#6123=CARTESIAN_POINT('Ctrl Pts',(48.706329375,29.8958333401613,-13.0508216223155));
#6124=CARTESIAN_POINT('Ctrl Pts',(48.706329375,29.687500006828,1.293339198242E-14));
#6125=CARTESIAN_POINT('Ctrl Pts',(48.706329375,29.4791666734946,13.0508216223155));
#6126=CARTESIAN_POINT('Ctrl Pts',(42.1809185638422,29.2708333401613,24.3531646875));
#6127=CARTESIAN_POINT('Ctrl Pts',(35.6555077526845,29.062500006828,35.6555077526845));
#6128=CARTESIAN_POINT('Ctrl Pts',(24.3531646875,28.8541666734946,42.1809185638422));
#6129=CARTESIAN_POINT('Ctrl Pts',(13.0508216223155,28.6458333401613,48.706329375));
#6130=CARTESIAN_POINT('Ctrl Pts',(-9.95098946405443E-15,28.437500006828,
48.706329375));
#6131=CARTESIAN_POINT('Ctrl Pts',(-13.0508216223155,28.2291666734946,48.706329375));
#6132=CARTESIAN_POINT('Ctrl Pts',(-24.3531646875,28.0208333401613,42.1809185638423));
#6133=CARTESIAN_POINT('Ctrl Pts',(-35.6555077526845,27.812500006828,35.6555077526845));
#6134=CARTESIAN_POINT('Ctrl Pts',(-42.1809185638422,27.6041666734946,24.3531646875));
#6135=CARTESIAN_POINT('Ctrl Pts',(-48.706329375,27.3958333401613,13.0508216223155));
#6136=CARTESIAN_POINT('Ctrl Pts',(-48.706329375,27.187500006828,-1.8898197019151E-14));
#6137=CARTESIAN_POINT('',(48.5725845633798,54.6293483229262,3.60701400320328));
#6138=CARTESIAN_POINT('Ctrl Pts',(45.858362923034,53.0633913333999,3.60701400320327));
#6139=CARTESIAN_POINT('Ctrl Pts',(46.089925771934,53.1969849680263,3.60701400320327));
#6140=CARTESIAN_POINT('Ctrl Pts',(46.5530501979845,53.4641744416604,3.60701400320329));
#6141=CARTESIAN_POINT('Ctrl Pts',(47.0161721905706,53.7313681332063,3.60701400320326));
#6142=CARTESIAN_POINT('Ctrl Pts',(47.689351986232,54.1197565257476,3.60701400320326));
#6143=CARTESIAN_POINT('Ctrl Pts',(48.1309692507095,54.3745507329179,3.60701400320328));
#6144=CARTESIAN_POINT('Ctrl Pts',(48.5725845633798,54.6293483229262,3.60701400320328));
#6145=CARTESIAN_POINT('',(3.612927284338,53.4957479656467,48.5721450795008));
#6146=CARTESIAN_POINT('Ctrl Pts',(48.5725845633798,54.6293483229262,3.60701400320328));
#6147=CARTESIAN_POINT('Ctrl Pts',(47.7480251419552,54.4485714020251,14.7106532430575));
#6148=CARTESIAN_POINT('Ctrl Pts',(42.1809185638422,54.2708333401613,24.3531646875));
#6149=CARTESIAN_POINT('Ctrl Pts',(35.6555077526845,54.062500006828,35.6555077526845));
#6150=CARTESIAN_POINT('Ctrl Pts',(24.3531646875,53.8541666734946,42.1809185638422));
#6151=CARTESIAN_POINT('Ctrl Pts',(14.7133549689477,53.6764784118853,47.7464652997852));
#6152=CARTESIAN_POINT('Ctrl Pts',(3.612927284338,53.4957479656467,48.5721450795008));
#6153=CARTESIAN_POINT('Ctrl Pts',(3.612927284338,53.4957479656467,48.5721450795008));
#6154=CARTESIAN_POINT('Ctrl Pts',(3.612927284338,53.3625660950884,48.3403451622817));
#6155=CARTESIAN_POINT('Ctrl Pts',(3.612927284338,53.2293911846469,48.1085412459393));
#6156=CARTESIAN_POINT('Ctrl Pts',(3.612927284338,52.9630558994543,47.6449250631479));
#6157=CARTESIAN_POINT('Ctrl Pts',(3.61292728433799,52.8298955244832,47.4131127965212));
#6158=CARTESIAN_POINT('Ctrl Pts',(3.61292728433799,52.6967427432646,47.1812961682826));
#6159=CARTESIAN_POINT('Ctrl Pts',(3.61292728433799,52.4433704509922,46.7401795055578));
#6160=CARTESIAN_POINT('Ctrl Pts',(3.612927284338,52.1900256371662,46.2990470581854));
#6161=CARTESIAN_POINT('Ctrl Pts',(3.612927284338,51.936710750803,45.8578974271399));
#6162=CARTESIAN_POINT('Ctrl Pts',(-46.,55.6250000136559,0.));
#6163=CARTESIAN_POINT('Ctrl Pts',(-46.,55.4166666803226,-12.3256628518316));
#6164=CARTESIAN_POINT('Ctrl Pts',(-39.8371685740842,55.2083333469893,-23.));
#6165=CARTESIAN_POINT('Ctrl Pts',(-33.6743371481684,55.0000000136559,-33.6743371481684));
#6166=CARTESIAN_POINT('Ctrl Pts',(-23.,54.7916666803226,-39.8371685740842));
#6167=CARTESIAN_POINT('Ctrl Pts',(-12.3256628518317,54.5833333469893,-46.));
#6168=CARTESIAN_POINT('Ctrl Pts',(-2.81668763803891E-15,54.3750000136559,
-46.));
#6169=CARTESIAN_POINT('Ctrl Pts',(12.3256628518316,54.1666666803226,-46.));
#6170=CARTESIAN_POINT('Ctrl Pts',(23.,53.9583333469893,-39.8371685740842));
#6171=CARTESIAN_POINT('Ctrl Pts',(33.6743371481683,53.7500000136559,-33.6743371481684));
#6172=CARTESIAN_POINT('Ctrl Pts',(39.8371685740842,53.5416666803226,-23.));
#6173=CARTESIAN_POINT('Ctrl Pts',(46.,53.3333333469893,-12.3256628518317));
#6174=CARTESIAN_POINT('Ctrl Pts',(46.,53.1250000136559,-5.63337527607782E-15));
#6175=CARTESIAN_POINT('Ctrl Pts',(46.,52.9166666803226,12.3256628518316));
#6176=CARTESIAN_POINT('Ctrl Pts',(39.8371685740842,52.7083333469893,23.));
#6177=CARTESIAN_POINT('Ctrl Pts',(33.6743371481684,52.5000000136559,33.6743371481683));
#6178=CARTESIAN_POINT('Ctrl Pts',(23.,52.2916666803226,39.8371685740842));
#6179=CARTESIAN_POINT('Ctrl Pts',(12.3256628518317,52.0833333469893,46.));
#6180=CARTESIAN_POINT('Ctrl Pts',(8.45006291411674E-15,51.8750000136559,
46.));
#6181=CARTESIAN_POINT('Ctrl Pts',(-12.3256628518316,51.6666666803226,46.));
#6182=CARTESIAN_POINT('Ctrl Pts',(-23.,51.4583333469893,39.8371685740842));
#6183=CARTESIAN_POINT('Ctrl Pts',(-33.6743371481683,51.2500000136559,33.6743371481684));
#6184=CARTESIAN_POINT('Ctrl Pts',(-39.8371685740842,51.0416666803226,23.));
#6185=CARTESIAN_POINT('Ctrl Pts',(-46.,50.8333333469893,12.3256628518317));
#6186=CARTESIAN_POINT('Ctrl Pts',(-46.,50.6250000136559,0.));
#6187=CARTESIAN_POINT('Ctrl Pts',(-46.,50.4166666803226,-12.3256628518316));
#6188=CARTESIAN_POINT('Ctrl Pts',(-39.8371685740842,50.2083333469893,-23.));
#6189=CARTESIAN_POINT('Ctrl Pts',(-33.6743371481684,50.0000000136559,-33.6743371481684));
#6190=CARTESIAN_POINT('Ctrl Pts',(-23.,49.7916666803226,-39.8371685740842));
#6191=CARTESIAN_POINT('Ctrl Pts',(-12.3256628518317,49.5833333469893,-46.));
#6192=CARTESIAN_POINT('Ctrl Pts',(-2.81668763803891E-15,49.3750000136559,
-46.));
#6193=CARTESIAN_POINT('Ctrl Pts',(12.3256628518316,49.1666666803226,-46.));
#6194=CARTESIAN_POINT('Ctrl Pts',(23.,48.9583333469893,-39.8371685740842));
#6195=CARTESIAN_POINT('Ctrl Pts',(33.6743371481683,48.7500000136559,-33.6743371481684));
#6196=CARTESIAN_POINT('Ctrl Pts',(39.8371685740842,48.5416666803226,-23.));
#6197=CARTESIAN_POINT('Ctrl Pts',(46.,48.3333333469893,-12.3256628518317));
#6198=CARTESIAN_POINT('Ctrl Pts',(46.,48.1250000136559,-5.63337527607782E-15));
#6199=CARTESIAN_POINT('Ctrl Pts',(46.,47.9166666803226,12.3256628518316));
#6200=CARTESIAN_POINT('Ctrl Pts',(39.8371685740842,47.7083333469893,23.));
#6201=CARTESIAN_POINT('Ctrl Pts',(33.6743371481684,47.5000000136559,33.6743371481683));
#6202=CARTESIAN_POINT('Ctrl Pts',(23.,47.2916666803226,39.8371685740842));
#6203=CARTESIAN_POINT('Ctrl Pts',(12.3256628518317,47.0833333469893,46.));
#6204=CARTESIAN_POINT('Ctrl Pts',(8.45006291411674E-15,46.8750000136559,
46.));
#6205=CARTESIAN_POINT('Ctrl Pts',(-12.3256628518316,46.6666666803226,46.));
#6206=CARTESIAN_POINT('Ctrl Pts',(-23.,46.4583333469893,39.8371685740842));
#6207=CARTESIAN_POINT('Ctrl Pts',(-33.6743371481683,46.2500000136559,33.6743371481684));
#6208=CARTESIAN_POINT('Ctrl Pts',(-39.8371685740842,46.0416666803226,23.));
#6209=CARTESIAN_POINT('Ctrl Pts',(-46.,45.8333333469892,12.3256628518317));
#6210=CARTESIAN_POINT('Ctrl Pts',(-46.,45.6250000136559,0.));
#6211=CARTESIAN_POINT('Ctrl Pts',(-46.,45.4166666803226,-12.3256628518316));
#6212=CARTESIAN_POINT('Ctrl Pts',(-39.8371685740842,45.2083333469893,-23.));
#6213=CARTESIAN_POINT('Ctrl Pts',(-33.6743371481684,45.0000000136559,-33.6743371481684));
#6214=CARTESIAN_POINT('Ctrl Pts',(-23.,44.7916666803226,-39.8371685740842));
#6215=CARTESIAN_POINT('Ctrl Pts',(-12.3256628518317,44.5833333469893,-46.));
#6216=CARTESIAN_POINT('Ctrl Pts',(-2.81668763803891E-15,44.3750000136559,
-46.));
#6217=CARTESIAN_POINT('Ctrl Pts',(12.3256628518316,44.1666666803226,-46.));
#6218=CARTESIAN_POINT('Ctrl Pts',(23.,43.9583333469893,-39.8371685740842));
#6219=CARTESIAN_POINT('Ctrl Pts',(33.6743371481683,43.7500000136559,-33.6743371481684));
#6220=CARTESIAN_POINT('Ctrl Pts',(39.8371685740842,43.5416666803226,-23.));
#6221=CARTESIAN_POINT('Ctrl Pts',(46.,43.3333333469893,-12.3256628518317));
#6222=CARTESIAN_POINT('Ctrl Pts',(46.,43.1250000136559,-5.63337527607782E-15));
#6223=CARTESIAN_POINT('Ctrl Pts',(46.,42.9166666803226,12.3256628518316));
#6224=CARTESIAN_POINT('Ctrl Pts',(39.8371685740842,42.7083333469893,23.));
#6225=CARTESIAN_POINT('Ctrl Pts',(33.6743371481684,42.5000000136559,33.6743371481683));
#6226=CARTESIAN_POINT('Ctrl Pts',(23.,42.2916666803226,39.8371685740842));
#6227=CARTESIAN_POINT('Ctrl Pts',(12.3256628518317,42.0833333469893,46.));
#6228=CARTESIAN_POINT('Ctrl Pts',(8.45006291411674E-15,41.8750000136559,
46.));
#6229=CARTESIAN_POINT('Ctrl Pts',(-12.3256628518316,41.6666666803226,46.));
#6230=CARTESIAN_POINT('Ctrl Pts',(-23.,41.4583333469893,39.8371685740842));
#6231=CARTESIAN_POINT('Ctrl Pts',(-33.6743371481683,41.2500000136559,33.6743371481684));
#6232=CARTESIAN_POINT('Ctrl Pts',(-39.8371685740842,41.0416666803226,23.));
#6233=CARTESIAN_POINT('Ctrl Pts',(-46.,40.8333333469893,12.3256628518317));
#6234=CARTESIAN_POINT('Ctrl Pts',(-46.,40.6250000136559,0.));
#6235=CARTESIAN_POINT('Ctrl Pts',(-46.,40.4166666803226,-12.3256628518316));
#6236=CARTESIAN_POINT('Ctrl Pts',(-39.8371685740842,40.2083333469893,-23.));
#6237=CARTESIAN_POINT('Ctrl Pts',(-33.6743371481684,40.0000000136559,-33.6743371481684));
#6238=CARTESIAN_POINT('Ctrl Pts',(-23.,39.7916666803226,-39.8371685740842));
#6239=CARTESIAN_POINT('Ctrl Pts',(-12.3256628518317,39.5833333469893,-46.));
#6240=CARTESIAN_POINT('Ctrl Pts',(-2.81668763803891E-15,39.3750000136559,
-46.));
#6241=CARTESIAN_POINT('Ctrl Pts',(12.3256628518316,39.1666666803226,-46.));
#6242=CARTESIAN_POINT('Ctrl Pts',(23.,38.9583333469893,-39.8371685740842));
#6243=CARTESIAN_POINT('Ctrl Pts',(33.6743371481683,38.7500000136559,-33.6743371481684));
#6244=CARTESIAN_POINT('Ctrl Pts',(39.8371685740842,38.5416666803226,-23.));
#6245=CARTESIAN_POINT('Ctrl Pts',(46.,38.3333333469893,-12.3256628518317));
#6246=CARTESIAN_POINT('Ctrl Pts',(46.,38.1250000136559,-5.63337527607782E-15));
#6247=CARTESIAN_POINT('Ctrl Pts',(46.,37.9166666803226,12.3256628518316));
#6248=CARTESIAN_POINT('Ctrl Pts',(39.8371685740842,37.7083333469893,23.));
#6249=CARTESIAN_POINT('Ctrl Pts',(33.6743371481684,37.5000000136559,33.6743371481683));
#6250=CARTESIAN_POINT('Ctrl Pts',(23.,37.2916666803226,39.8371685740842));
#6251=CARTESIAN_POINT('Ctrl Pts',(12.3256628518317,37.0833333469893,46.));
#6252=CARTESIAN_POINT('Ctrl Pts',(8.45006291411674E-15,36.8750000136559,
46.));
#6253=CARTESIAN_POINT('Ctrl Pts',(-12.3256628518316,36.6666666803226,46.));
#6254=CARTESIAN_POINT('Ctrl Pts',(-23.,36.4583333469893,39.8371685740842));
#6255=CARTESIAN_POINT('Ctrl Pts',(-33.6743371481683,36.2500000136559,33.6743371481684));
#6256=CARTESIAN_POINT('Ctrl Pts',(-39.8371685740842,36.0416666803226,23.));
#6257=CARTESIAN_POINT('Ctrl Pts',(-46.,35.8333333469893,12.3256628518317));
#6258=CARTESIAN_POINT('Ctrl Pts',(-46.,35.6250000136559,0.));
#6259=CARTESIAN_POINT('Ctrl Pts',(-46.,35.4166666803226,-12.3256628518316));
#6260=CARTESIAN_POINT('Ctrl Pts',(-39.8371685740842,35.2083333469893,-23.));
#6261=CARTESIAN_POINT('Ctrl Pts',(-33.6743371481684,35.0000000136559,-33.6743371481684));
#6262=CARTESIAN_POINT('Ctrl Pts',(-23.,34.7916666803226,-39.8371685740842));
#6263=CARTESIAN_POINT('Ctrl Pts',(-12.3256628518317,34.5833333469893,-46.));
#6264=CARTESIAN_POINT('Ctrl Pts',(-2.81668763803891E-15,34.3750000136559,
-46.));
#6265=CARTESIAN_POINT('Ctrl Pts',(12.3256628518316,34.1666666803226,-46.));
#6266=CARTESIAN_POINT('Ctrl Pts',(23.,33.9583333469893,-39.8371685740842));
#6267=CARTESIAN_POINT('Ctrl Pts',(33.6743371481683,33.7500000136559,-33.6743371481684));
#6268=CARTESIAN_POINT('Ctrl Pts',(39.8371685740842,33.5416666803226,-23.));
#6269=CARTESIAN_POINT('Ctrl Pts',(46.,33.3333333469893,-12.3256628518317));
#6270=CARTESIAN_POINT('Ctrl Pts',(46.,33.1250000136559,-5.63337527607782E-15));
#6271=CARTESIAN_POINT('Ctrl Pts',(46.,32.9166666803226,12.3256628518316));
#6272=CARTESIAN_POINT('Ctrl Pts',(39.8371685740842,32.7083333469893,23.));
#6273=CARTESIAN_POINT('Ctrl Pts',(33.6743371481684,32.5000000136559,33.6743371481683));
#6274=CARTESIAN_POINT('Ctrl Pts',(23.,32.2916666803226,39.8371685740842));
#6275=CARTESIAN_POINT('Ctrl Pts',(12.3256628518317,32.0833333469893,46.));
#6276=CARTESIAN_POINT('Ctrl Pts',(8.45006291411674E-15,31.8750000136559,
46.));
#6277=CARTESIAN_POINT('Ctrl Pts',(-12.3256628518316,31.6666666803226,46.));
#6278=CARTESIAN_POINT('Ctrl Pts',(-23.,31.4583333469893,39.8371685740842));
#6279=CARTESIAN_POINT('Ctrl Pts',(-33.6743371481683,31.2500000136559,33.6743371481684));
#6280=CARTESIAN_POINT('Ctrl Pts',(-39.8371685740842,31.0416666803226,23.));
#6281=CARTESIAN_POINT('Ctrl Pts',(-46.,30.8333333469893,12.3256628518317));
#6282=CARTESIAN_POINT('Ctrl Pts',(-46.,30.6250000136559,0.));
#6283=CARTESIAN_POINT('Ctrl Pts',(-46.,30.4166666803226,-12.3256628518316));
#6284=CARTESIAN_POINT('Ctrl Pts',(-39.8371685740842,30.2083333469893,-23.));
#6285=CARTESIAN_POINT('Ctrl Pts',(-33.6743371481684,30.0000000136559,-33.6743371481684));
#6286=CARTESIAN_POINT('Ctrl Pts',(-23.,29.7916666803226,-39.8371685740842));
#6287=CARTESIAN_POINT('Ctrl Pts',(-12.3256628518317,29.5833333469893,-46.));
#6288=CARTESIAN_POINT('Ctrl Pts',(-2.81668763803891E-15,29.3750000136559,
-46.));
#6289=CARTESIAN_POINT('Ctrl Pts',(12.3256628518316,29.1666666803226,-46.));
#6290=CARTESIAN_POINT('Ctrl Pts',(23.,28.9583333469893,-39.8371685740842));
#6291=CARTESIAN_POINT('Ctrl Pts',(33.6743371481683,28.7500000136559,-33.6743371481684));
#6292=CARTESIAN_POINT('Ctrl Pts',(39.8371685740842,28.5416666803226,-23.));
#6293=CARTESIAN_POINT('Ctrl Pts',(46.,28.3333333469893,-12.3256628518317));
#6294=CARTESIAN_POINT('Ctrl Pts',(46.,28.1250000136559,-5.63337527607782E-15));
#6295=CARTESIAN_POINT('Ctrl Pts',(46.,27.9166666803226,12.3256628518316));
#6296=CARTESIAN_POINT('Ctrl Pts',(39.8371685740842,27.7083333469893,23.));
#6297=CARTESIAN_POINT('Ctrl Pts',(33.6743371481684,27.5000000136559,33.6743371481683));
#6298=CARTESIAN_POINT('Ctrl Pts',(23.,27.2916666803226,39.8371685740842));
#6299=CARTESIAN_POINT('Ctrl Pts',(12.3256628518317,27.0833333469893,46.));
#6300=CARTESIAN_POINT('Ctrl Pts',(8.45006291411674E-15,26.8750000136559,
46.));
#6301=CARTESIAN_POINT('Ctrl Pts',(-12.3256628518316,26.6666666803226,46.));
#6302=CARTESIAN_POINT('Ctrl Pts',(-23.,26.4583333469893,39.8371685740842));
#6303=CARTESIAN_POINT('Ctrl Pts',(-33.6743371481683,26.2500000136559,33.6743371481684));
#6304=CARTESIAN_POINT('Ctrl Pts',(-39.8371685740842,26.0416666803226,23.));
#6305=CARTESIAN_POINT('Ctrl Pts',(-46.,25.8333333469893,12.3256628518317));
#6306=CARTESIAN_POINT('Ctrl Pts',(-46.,25.6250000136559,0.));
#6307=CARTESIAN_POINT('Ctrl Pts',(-48.706329375,57.187500006828,-1.8898197019151E-14));
#6308=CARTESIAN_POINT('Ctrl Pts',(-48.706329375,56.9791666734946,-13.0508216223155));
#6309=CARTESIAN_POINT('Ctrl Pts',(-42.1809185638422,56.7708333401613,-24.3531646875));
#6310=CARTESIAN_POINT('Ctrl Pts',(-35.6555077526845,56.562500006828,-35.6555077526845));
#6311=CARTESIAN_POINT('Ctrl Pts',(-24.3531646875,56.3541666734946,-42.1809185638423));
#6312=CARTESIAN_POINT('Ctrl Pts',(-13.0508216223155,56.1458333401613,-48.706329375));
#6313=CARTESIAN_POINT('Ctrl Pts',(1.59157945007855E-14,55.937500006828,
-48.706329375));
#6314=CARTESIAN_POINT('Ctrl Pts',(13.0508216223155,55.7291666734946,-48.706329375));
#6315=CARTESIAN_POINT('Ctrl Pts',(24.3531646875,55.5208333401613,-42.1809185638422));
#6316=CARTESIAN_POINT('Ctrl Pts',(35.6555077526845,55.312500006828,-35.6555077526845));
#6317=CARTESIAN_POINT('Ctrl Pts',(42.1809185638422,55.1041666734946,-24.3531646875));
#6318=CARTESIAN_POINT('Ctrl Pts',(48.706329375,54.8958333401613,-13.0508216223155));
#6319=CARTESIAN_POINT('Ctrl Pts',(48.706329375,54.687500006828,1.293339198242E-14));
#6320=CARTESIAN_POINT('Ctrl Pts',(48.706329375,54.4791666734946,13.0508216223155));
#6321=CARTESIAN_POINT('Ctrl Pts',(42.1809185638422,54.2708333401613,24.3531646875));
#6322=CARTESIAN_POINT('Ctrl Pts',(35.6555077526845,54.062500006828,35.6555077526845));
#6323=CARTESIAN_POINT('Ctrl Pts',(24.3531646875,53.8541666734946,42.1809185638422));
#6324=CARTESIAN_POINT('Ctrl Pts',(13.0508216223155,53.6458333401613,48.706329375));
#6325=CARTESIAN_POINT('Ctrl Pts',(-9.95098946405443E-15,53.437500006828,
48.706329375));
#6326=CARTESIAN_POINT('Ctrl Pts',(-13.0508216223155,53.2291666734946,48.706329375));
#6327=CARTESIAN_POINT('Ctrl Pts',(-24.3531646875,53.0208333401613,42.1809185638423));
#6328=CARTESIAN_POINT('Ctrl Pts',(-35.6555077526845,52.812500006828,35.6555077526845));
#6329=CARTESIAN_POINT('Ctrl Pts',(-42.1809185638422,52.6041666734946,24.3531646875));
#6330=CARTESIAN_POINT('Ctrl Pts',(-48.706329375,52.3958333401613,13.0508216223155));
#6331=CARTESIAN_POINT('Ctrl Pts',(-48.706329375,52.187500006828,-1.8898197019151E-14));
#6332=CARTESIAN_POINT('Ctrl Pts',(-48.706329375,51.9791666734946,-13.0508216223155));
#6333=CARTESIAN_POINT('Ctrl Pts',(-42.1809185638422,51.7708333401613,-24.3531646875));
#6334=CARTESIAN_POINT('Ctrl Pts',(-35.6555077526845,51.562500006828,-35.6555077526845));
#6335=CARTESIAN_POINT('Ctrl Pts',(-24.3531646875,51.3541666734946,-42.1809185638423));
#6336=CARTESIAN_POINT('Ctrl Pts',(-13.0508216223155,51.1458333401613,-48.706329375));
#6337=CARTESIAN_POINT('Ctrl Pts',(1.59157945007855E-14,50.937500006828,
-48.706329375));
#6338=CARTESIAN_POINT('Ctrl Pts',(13.0508216223155,50.7291666734946,-48.706329375));
#6339=CARTESIAN_POINT('Ctrl Pts',(24.3531646875,50.5208333401613,-42.1809185638422));
#6340=CARTESIAN_POINT('Ctrl Pts',(35.6555077526845,50.312500006828,-35.6555077526845));
#6341=CARTESIAN_POINT('Ctrl Pts',(42.1809185638422,50.1041666734946,-24.3531646875));
#6342=CARTESIAN_POINT('Ctrl Pts',(48.706329375,49.8958333401613,-13.0508216223155));
#6343=CARTESIAN_POINT('Ctrl Pts',(48.706329375,49.687500006828,1.293339198242E-14));
#6344=CARTESIAN_POINT('Ctrl Pts',(48.706329375,49.4791666734946,13.0508216223155));
#6345=CARTESIAN_POINT('Ctrl Pts',(42.1809185638422,49.2708333401613,24.3531646875));
#6346=CARTESIAN_POINT('Ctrl Pts',(35.6555077526845,49.062500006828,35.6555077526845));
#6347=CARTESIAN_POINT('Ctrl Pts',(24.3531646875,48.8541666734946,42.1809185638422));
#6348=CARTESIAN_POINT('Ctrl Pts',(13.0508216223155,48.6458333401613,48.706329375));
#6349=CARTESIAN_POINT('Ctrl Pts',(-9.95098946405443E-15,48.437500006828,
48.706329375));
#6350=CARTESIAN_POINT('Ctrl Pts',(-13.0508216223155,48.2291666734946,48.706329375));
#6351=CARTESIAN_POINT('Ctrl Pts',(-24.3531646875,48.0208333401613,42.1809185638423));
#6352=CARTESIAN_POINT('Ctrl Pts',(-35.6555077526845,47.812500006828,35.6555077526845));
#6353=CARTESIAN_POINT('Ctrl Pts',(-42.1809185638422,47.6041666734946,24.3531646875));
#6354=CARTESIAN_POINT('Ctrl Pts',(-48.706329375,47.3958333401613,13.0508216223155));
#6355=CARTESIAN_POINT('Ctrl Pts',(-48.706329375,47.187500006828,-1.8898197019151E-14));
#6356=CARTESIAN_POINT('Ctrl Pts',(-48.706329375,46.9791666734946,-13.0508216223155));
#6357=CARTESIAN_POINT('Ctrl Pts',(-42.1809185638422,46.7708333401613,-24.3531646875));
#6358=CARTESIAN_POINT('Ctrl Pts',(-35.6555077526845,46.562500006828,-35.6555077526845));
#6359=CARTESIAN_POINT('Ctrl Pts',(-24.3531646875,46.3541666734946,-42.1809185638423));
#6360=CARTESIAN_POINT('Ctrl Pts',(-13.0508216223155,46.1458333401613,-48.706329375));
#6361=CARTESIAN_POINT('Ctrl Pts',(1.59157945007855E-14,45.937500006828,
-48.706329375));
#6362=CARTESIAN_POINT('Ctrl Pts',(13.0508216223155,45.7291666734946,-48.706329375));
#6363=CARTESIAN_POINT('Ctrl Pts',(24.3531646875,45.5208333401613,-42.1809185638422));
#6364=CARTESIAN_POINT('Ctrl Pts',(35.6555077526845,45.312500006828,-35.6555077526845));
#6365=CARTESIAN_POINT('Ctrl Pts',(42.1809185638422,45.1041666734946,-24.3531646875));
#6366=CARTESIAN_POINT('Ctrl Pts',(48.706329375,44.8958333401613,-13.0508216223155));
#6367=CARTESIAN_POINT('Ctrl Pts',(48.706329375,44.687500006828,1.293339198242E-14));
#6368=CARTESIAN_POINT('Ctrl Pts',(48.706329375,44.4791666734946,13.0508216223155));
#6369=CARTESIAN_POINT('Ctrl Pts',(42.1809185638422,44.2708333401613,24.3531646875));
#6370=CARTESIAN_POINT('Ctrl Pts',(35.6555077526845,44.062500006828,35.6555077526845));
#6371=CARTESIAN_POINT('Ctrl Pts',(24.3531646875,43.8541666734946,42.1809185638422));
#6372=CARTESIAN_POINT('Ctrl Pts',(13.0508216223155,43.6458333401613,48.706329375));
#6373=CARTESIAN_POINT('Ctrl Pts',(-9.95098946405443E-15,43.437500006828,
48.706329375));
#6374=CARTESIAN_POINT('Ctrl Pts',(-13.0508216223155,43.2291666734946,48.706329375));
#6375=CARTESIAN_POINT('Ctrl Pts',(-24.3531646875,43.0208333401613,42.1809185638423));
#6376=CARTESIAN_POINT('Ctrl Pts',(-35.6555077526845,42.812500006828,35.6555077526845));
#6377=CARTESIAN_POINT('Ctrl Pts',(-42.1809185638422,42.6041666734946,24.3531646875));
#6378=CARTESIAN_POINT('Ctrl Pts',(-48.706329375,42.3958333401613,13.0508216223155));
#6379=CARTESIAN_POINT('Ctrl Pts',(-48.706329375,42.187500006828,-1.8898197019151E-14));
#6380=CARTESIAN_POINT('Ctrl Pts',(-48.706329375,41.9791666734946,-13.0508216223155));
#6381=CARTESIAN_POINT('Ctrl Pts',(-42.1809185638422,41.7708333401613,-24.3531646875));
#6382=CARTESIAN_POINT('Ctrl Pts',(-35.6555077526845,41.562500006828,-35.6555077526845));
#6383=CARTESIAN_POINT('Ctrl Pts',(-24.3531646875,41.3541666734946,-42.1809185638423));
#6384=CARTESIAN_POINT('Ctrl Pts',(-13.0508216223155,41.1458333401613,-48.706329375));
#6385=CARTESIAN_POINT('Ctrl Pts',(1.59157945007855E-14,40.937500006828,
-48.706329375));
#6386=CARTESIAN_POINT('Ctrl Pts',(13.0508216223155,40.7291666734946,-48.706329375));
#6387=CARTESIAN_POINT('Ctrl Pts',(24.3531646875,40.5208333401613,-42.1809185638422));
#6388=CARTESIAN_POINT('Ctrl Pts',(35.6555077526845,40.312500006828,-35.6555077526845));
#6389=CARTESIAN_POINT('Ctrl Pts',(42.1809185638422,40.1041666734946,-24.3531646875));
#6390=CARTESIAN_POINT('Ctrl Pts',(48.706329375,39.8958333401613,-13.0508216223155));
#6391=CARTESIAN_POINT('Ctrl Pts',(48.706329375,39.687500006828,1.293339198242E-14));
#6392=CARTESIAN_POINT('Ctrl Pts',(48.706329375,39.4791666734946,13.0508216223155));
#6393=CARTESIAN_POINT('Ctrl Pts',(42.1809185638422,39.2708333401613,24.3531646875));
#6394=CARTESIAN_POINT('Ctrl Pts',(35.6555077526845,39.062500006828,35.6555077526845));
#6395=CARTESIAN_POINT('Ctrl Pts',(24.3531646875,38.8541666734946,42.1809185638422));
#6396=CARTESIAN_POINT('Ctrl Pts',(13.0508216223155,38.6458333401613,48.706329375));
#6397=CARTESIAN_POINT('Ctrl Pts',(-9.95098946405443E-15,38.437500006828,
48.706329375));
#6398=CARTESIAN_POINT('Ctrl Pts',(-13.0508216223155,38.2291666734946,48.706329375));
#6399=CARTESIAN_POINT('Ctrl Pts',(-24.3531646875,38.0208333401613,42.1809185638423));
#6400=CARTESIAN_POINT('Ctrl Pts',(-35.6555077526845,37.812500006828,35.6555077526845));
#6401=CARTESIAN_POINT('Ctrl Pts',(-42.1809185638422,37.6041666734946,24.3531646875));
#6402=CARTESIAN_POINT('Ctrl Pts',(-48.706329375,37.3958333401613,13.0508216223155));
#6403=CARTESIAN_POINT('Ctrl Pts',(-48.706329375,37.187500006828,-1.8898197019151E-14));
#6404=CARTESIAN_POINT('Ctrl Pts',(-48.706329375,36.9791666734946,-13.0508216223155));
#6405=CARTESIAN_POINT('Ctrl Pts',(-42.1809185638422,36.7708333401613,-24.3531646875));
#6406=CARTESIAN_POINT('Ctrl Pts',(-35.6555077526845,36.562500006828,-35.6555077526845));
#6407=CARTESIAN_POINT('Ctrl Pts',(-24.3531646875,36.3541666734946,-42.1809185638423));
#6408=CARTESIAN_POINT('Ctrl Pts',(-13.0508216223155,36.1458333401613,-48.706329375));
#6409=CARTESIAN_POINT('Ctrl Pts',(1.59157945007855E-14,35.937500006828,
-48.706329375));
#6410=CARTESIAN_POINT('Ctrl Pts',(13.0508216223155,35.7291666734946,-48.706329375));
#6411=CARTESIAN_POINT('Ctrl Pts',(24.3531646875,35.5208333401613,-42.1809185638422));
#6412=CARTESIAN_POINT('Ctrl Pts',(35.6555077526845,35.312500006828,-35.6555077526845));
#6413=CARTESIAN_POINT('Ctrl Pts',(42.1809185638422,35.1041666734946,-24.3531646875));
#6414=CARTESIAN_POINT('Ctrl Pts',(48.706329375,34.8958333401613,-13.0508216223155));
#6415=CARTESIAN_POINT('Ctrl Pts',(48.706329375,34.687500006828,1.293339198242E-14));
#6416=CARTESIAN_POINT('Ctrl Pts',(48.706329375,34.4791666734946,13.0508216223155));
#6417=CARTESIAN_POINT('Ctrl Pts',(42.1809185638422,34.2708333401613,24.3531646875));
#6418=CARTESIAN_POINT('Ctrl Pts',(35.6555077526845,34.062500006828,35.6555077526845));
#6419=CARTESIAN_POINT('Ctrl Pts',(24.3531646875,33.8541666734946,42.1809185638422));
#6420=CARTESIAN_POINT('Ctrl Pts',(13.0508216223155,33.6458333401613,48.706329375));
#6421=CARTESIAN_POINT('Ctrl Pts',(-9.95098946405443E-15,33.437500006828,
48.706329375));
#6422=CARTESIAN_POINT('Ctrl Pts',(-13.0508216223155,33.2291666734946,48.706329375));
#6423=CARTESIAN_POINT('Ctrl Pts',(-24.3531646875,33.0208333401613,42.1809185638423));
#6424=CARTESIAN_POINT('Ctrl Pts',(-35.6555077526845,32.812500006828,35.6555077526845));
#6425=CARTESIAN_POINT('Ctrl Pts',(-42.1809185638422,32.6041666734946,24.3531646875));
#6426=CARTESIAN_POINT('Ctrl Pts',(-48.706329375,32.3958333401613,13.0508216223155));
#6427=CARTESIAN_POINT('Ctrl Pts',(-48.706329375,32.187500006828,-1.8898197019151E-14));
#6428=CARTESIAN_POINT('Ctrl Pts',(-48.706329375,31.9791666734946,-13.0508216223155));
#6429=CARTESIAN_POINT('Ctrl Pts',(-42.1809185638422,31.7708333401613,-24.3531646875));
#6430=CARTESIAN_POINT('Ctrl Pts',(-35.6555077526845,31.562500006828,-35.6555077526845));
#6431=CARTESIAN_POINT('Ctrl Pts',(-24.3531646875,31.3541666734946,-42.1809185638423));
#6432=CARTESIAN_POINT('Ctrl Pts',(-13.0508216223155,31.1458333401613,-48.706329375));
#6433=CARTESIAN_POINT('Ctrl Pts',(1.59157945007855E-14,30.937500006828,
-48.706329375));
#6434=CARTESIAN_POINT('Ctrl Pts',(13.0508216223155,30.7291666734946,-48.706329375));
#6435=CARTESIAN_POINT('Ctrl Pts',(24.3531646875,30.5208333401613,-42.1809185638422));
#6436=CARTESIAN_POINT('Ctrl Pts',(35.6555077526845,30.312500006828,-35.6555077526845));
#6437=CARTESIAN_POINT('Ctrl Pts',(42.1809185638422,30.1041666734946,-24.3531646875));
#6438=CARTESIAN_POINT('Ctrl Pts',(48.706329375,29.8958333401613,-13.0508216223155));
#6439=CARTESIAN_POINT('Ctrl Pts',(48.706329375,29.687500006828,1.293339198242E-14));
#6440=CARTESIAN_POINT('Ctrl Pts',(48.706329375,29.4791666734946,13.0508216223155));
#6441=CARTESIAN_POINT('Ctrl Pts',(42.1809185638422,29.2708333401613,24.3531646875));
#6442=CARTESIAN_POINT('Ctrl Pts',(35.6555077526845,29.062500006828,35.6555077526845));
#6443=CARTESIAN_POINT('Ctrl Pts',(24.3531646875,28.8541666734946,42.1809185638422));
#6444=CARTESIAN_POINT('Ctrl Pts',(13.0508216223155,28.6458333401613,48.706329375));
#6445=CARTESIAN_POINT('Ctrl Pts',(-9.95098946405443E-15,28.437500006828,
48.706329375));
#6446=CARTESIAN_POINT('Ctrl Pts',(-13.0508216223155,28.2291666734946,48.706329375));
#6447=CARTESIAN_POINT('Ctrl Pts',(-24.3531646875,28.0208333401613,42.1809185638423));
#6448=CARTESIAN_POINT('Ctrl Pts',(-35.6555077526845,27.812500006828,35.6555077526845));
#6449=CARTESIAN_POINT('Ctrl Pts',(-42.1809185638422,27.6041666734946,24.3531646875));
#6450=CARTESIAN_POINT('Ctrl Pts',(-48.706329375,27.3958333401613,13.0508216223155));
#6451=CARTESIAN_POINT('Ctrl Pts',(-48.706329375,27.187500006828,-1.8898197019151E-14));
#6452=CARTESIAN_POINT('',(3.612927284338,50.8792520480092,-48.5721450795008));
#6453=CARTESIAN_POINT('',(48.5134353784345,49.7574536451604,-4.33048599679671));
#6454=CARTESIAN_POINT('Ctrl Pts',(3.612927284338,50.8792520480092,-48.5721450795008));
#6455=CARTESIAN_POINT('Ctrl Pts',(14.7133549689477,50.6985216017706,-47.7464652997852));
#6456=CARTESIAN_POINT('Ctrl Pts',(24.3531646875,50.5208333401613,-42.1809185638422));
#6457=CARTESIAN_POINT('Ctrl Pts',(35.6555077526845,50.312500006828,-35.6555077526845));
#6458=CARTESIAN_POINT('Ctrl Pts',(42.1809185638422,50.1041666734946,-24.3531646875));
#6459=CARTESIAN_POINT('Ctrl Pts',(47.5573898704235,49.9325149229327,-15.0408432190651));
#6460=CARTESIAN_POINT('Ctrl Pts',(48.5134353784345,49.7574536451604,-4.33048599679671));
#6461=CARTESIAN_POINT('Origin',(-4513.80899810642,8003.28355107783,-4.33048626309052));
#6462=CARTESIAN_POINT('Ctrl Pts',(3.61292728433799,49.3132892765089,-45.8578974271399));
#6463=CARTESIAN_POINT('Ctrl Pts',(3.61292728433801,49.4468822859549,-46.089460636719));
#6464=CARTESIAN_POINT('Ctrl Pts',(3.612927284338,49.7140705280012,-46.5525857733052));
#6465=CARTESIAN_POINT('Ctrl Pts',(3.61292728433798,49.9812630238615,-47.0157084557285));
#6466=CARTESIAN_POINT('Ctrl Pts',(3.61292728433798,50.3696539378594,-47.6888965792834));
#6467=CARTESIAN_POINT('Ctrl Pts',(3.612927284338,50.624451287085,-48.1305218136162));
#6468=CARTESIAN_POINT('Ctrl Pts',(3.612927284338,50.8792520480092,-48.5721450795008));
#6469=CARTESIAN_POINT('Ctrl Pts',(-46.,55.6250000136559,0.));
#6470=CARTESIAN_POINT('Ctrl Pts',(-46.,55.4166666803226,-12.3256628518316));
#6471=CARTESIAN_POINT('Ctrl Pts',(-39.8371685740842,55.2083333469893,-23.));
#6472=CARTESIAN_POINT('Ctrl Pts',(-33.6743371481684,55.0000000136559,-33.6743371481684));
#6473=CARTESIAN_POINT('Ctrl Pts',(-23.,54.7916666803226,-39.8371685740842));
#6474=CARTESIAN_POINT('Ctrl Pts',(-12.3256628518317,54.5833333469893,-46.));
#6475=CARTESIAN_POINT('Ctrl Pts',(-2.81668763803891E-15,54.3750000136559,
-46.));
#6476=CARTESIAN_POINT('Ctrl Pts',(12.3256628518316,54.1666666803226,-46.));
#6477=CARTESIAN_POINT('Ctrl Pts',(23.,53.9583333469893,-39.8371685740842));
#6478=CARTESIAN_POINT('Ctrl Pts',(33.6743371481683,53.7500000136559,-33.6743371481684));
#6479=CARTESIAN_POINT('Ctrl Pts',(39.8371685740842,53.5416666803226,-23.));
#6480=CARTESIAN_POINT('Ctrl Pts',(46.,53.3333333469893,-12.3256628518317));
#6481=CARTESIAN_POINT('Ctrl Pts',(46.,53.1250000136559,-5.63337527607782E-15));
#6482=CARTESIAN_POINT('Ctrl Pts',(46.,52.9166666803226,12.3256628518316));
#6483=CARTESIAN_POINT('Ctrl Pts',(39.8371685740842,52.7083333469893,23.));
#6484=CARTESIAN_POINT('Ctrl Pts',(33.6743371481684,52.5000000136559,33.6743371481683));
#6485=CARTESIAN_POINT('Ctrl Pts',(23.,52.2916666803226,39.8371685740842));
#6486=CARTESIAN_POINT('Ctrl Pts',(12.3256628518317,52.0833333469893,46.));
#6487=CARTESIAN_POINT('Ctrl Pts',(8.45006291411674E-15,51.8750000136559,
46.));
#6488=CARTESIAN_POINT('Ctrl Pts',(-12.3256628518316,51.6666666803226,46.));
#6489=CARTESIAN_POINT('Ctrl Pts',(-23.,51.4583333469893,39.8371685740842));
#6490=CARTESIAN_POINT('Ctrl Pts',(-33.6743371481683,51.2500000136559,33.6743371481684));
#6491=CARTESIAN_POINT('Ctrl Pts',(-39.8371685740842,51.0416666803226,23.));
#6492=CARTESIAN_POINT('Ctrl Pts',(-46.,50.8333333469893,12.3256628518317));
#6493=CARTESIAN_POINT('Ctrl Pts',(-46.,50.6250000136559,0.));
#6494=CARTESIAN_POINT('Ctrl Pts',(-46.,50.4166666803226,-12.3256628518316));
#6495=CARTESIAN_POINT('Ctrl Pts',(-39.8371685740842,50.2083333469893,-23.));
#6496=CARTESIAN_POINT('Ctrl Pts',(-33.6743371481684,50.0000000136559,-33.6743371481684));
#6497=CARTESIAN_POINT('Ctrl Pts',(-23.,49.7916666803226,-39.8371685740842));
#6498=CARTESIAN_POINT('Ctrl Pts',(-12.3256628518317,49.5833333469893,-46.));
#6499=CARTESIAN_POINT('Ctrl Pts',(-2.81668763803891E-15,49.3750000136559,
-46.));
#6500=CARTESIAN_POINT('Ctrl Pts',(12.3256628518316,49.1666666803226,-46.));
#6501=CARTESIAN_POINT('Ctrl Pts',(23.,48.9583333469893,-39.8371685740842));
#6502=CARTESIAN_POINT('Ctrl Pts',(33.6743371481683,48.7500000136559,-33.6743371481684));
#6503=CARTESIAN_POINT('Ctrl Pts',(39.8371685740842,48.5416666803226,-23.));
#6504=CARTESIAN_POINT('Ctrl Pts',(46.,48.3333333469893,-12.3256628518317));
#6505=CARTESIAN_POINT('Ctrl Pts',(46.,48.1250000136559,-5.63337527607782E-15));
#6506=CARTESIAN_POINT('Ctrl Pts',(46.,47.9166666803226,12.3256628518316));
#6507=CARTESIAN_POINT('Ctrl Pts',(39.8371685740842,47.7083333469893,23.));
#6508=CARTESIAN_POINT('Ctrl Pts',(33.6743371481684,47.5000000136559,33.6743371481683));
#6509=CARTESIAN_POINT('Ctrl Pts',(23.,47.2916666803226,39.8371685740842));
#6510=CARTESIAN_POINT('Ctrl Pts',(12.3256628518317,47.0833333469893,46.));
#6511=CARTESIAN_POINT('Ctrl Pts',(8.45006291411674E-15,46.8750000136559,
46.));
#6512=CARTESIAN_POINT('Ctrl Pts',(-12.3256628518316,46.6666666803226,46.));
#6513=CARTESIAN_POINT('Ctrl Pts',(-23.,46.4583333469893,39.8371685740842));
#6514=CARTESIAN_POINT('Ctrl Pts',(-33.6743371481683,46.2500000136559,33.6743371481684));
#6515=CARTESIAN_POINT('Ctrl Pts',(-39.8371685740842,46.0416666803226,23.));
#6516=CARTESIAN_POINT('Ctrl Pts',(-46.,45.8333333469892,12.3256628518317));
#6517=CARTESIAN_POINT('Ctrl Pts',(-46.,45.6250000136559,0.));
#6518=CARTESIAN_POINT('Ctrl Pts',(-46.,45.4166666803226,-12.3256628518316));
#6519=CARTESIAN_POINT('Ctrl Pts',(-39.8371685740842,45.2083333469893,-23.));
#6520=CARTESIAN_POINT('Ctrl Pts',(-33.6743371481684,45.0000000136559,-33.6743371481684));
#6521=CARTESIAN_POINT('Ctrl Pts',(-23.,44.7916666803226,-39.8371685740842));
#6522=CARTESIAN_POINT('Ctrl Pts',(-12.3256628518317,44.5833333469893,-46.));
#6523=CARTESIAN_POINT('Ctrl Pts',(-2.81668763803891E-15,44.3750000136559,
-46.));
#6524=CARTESIAN_POINT('Ctrl Pts',(12.3256628518316,44.1666666803226,-46.));
#6525=CARTESIAN_POINT('Ctrl Pts',(23.,43.9583333469893,-39.8371685740842));
#6526=CARTESIAN_POINT('Ctrl Pts',(33.6743371481683,43.7500000136559,-33.6743371481684));
#6527=CARTESIAN_POINT('Ctrl Pts',(39.8371685740842,43.5416666803226,-23.));
#6528=CARTESIAN_POINT('Ctrl Pts',(46.,43.3333333469893,-12.3256628518317));
#6529=CARTESIAN_POINT('Ctrl Pts',(46.,43.1250000136559,-5.63337527607782E-15));
#6530=CARTESIAN_POINT('Ctrl Pts',(46.,42.9166666803226,12.3256628518316));
#6531=CARTESIAN_POINT('Ctrl Pts',(39.8371685740842,42.7083333469893,23.));
#6532=CARTESIAN_POINT('Ctrl Pts',(33.6743371481684,42.5000000136559,33.6743371481683));
#6533=CARTESIAN_POINT('Ctrl Pts',(23.,42.2916666803226,39.8371685740842));
#6534=CARTESIAN_POINT('Ctrl Pts',(12.3256628518317,42.0833333469893,46.));
#6535=CARTESIAN_POINT('Ctrl Pts',(8.45006291411674E-15,41.8750000136559,
46.));
#6536=CARTESIAN_POINT('Ctrl Pts',(-12.3256628518316,41.6666666803226,46.));
#6537=CARTESIAN_POINT('Ctrl Pts',(-23.,41.4583333469893,39.8371685740842));
#6538=CARTESIAN_POINT('Ctrl Pts',(-33.6743371481683,41.2500000136559,33.6743371481684));
#6539=CARTESIAN_POINT('Ctrl Pts',(-39.8371685740842,41.0416666803226,23.));
#6540=CARTESIAN_POINT('Ctrl Pts',(-46.,40.8333333469893,12.3256628518317));
#6541=CARTESIAN_POINT('Ctrl Pts',(-46.,40.6250000136559,0.));
#6542=CARTESIAN_POINT('Ctrl Pts',(-46.,40.4166666803226,-12.3256628518316));
#6543=CARTESIAN_POINT('Ctrl Pts',(-39.8371685740842,40.2083333469893,-23.));
#6544=CARTESIAN_POINT('Ctrl Pts',(-33.6743371481684,40.0000000136559,-33.6743371481684));
#6545=CARTESIAN_POINT('Ctrl Pts',(-23.,39.7916666803226,-39.8371685740842));
#6546=CARTESIAN_POINT('Ctrl Pts',(-12.3256628518317,39.5833333469893,-46.));
#6547=CARTESIAN_POINT('Ctrl Pts',(-2.81668763803891E-15,39.3750000136559,
-46.));
#6548=CARTESIAN_POINT('Ctrl Pts',(12.3256628518316,39.1666666803226,-46.));
#6549=CARTESIAN_POINT('Ctrl Pts',(23.,38.9583333469893,-39.8371685740842));
#6550=CARTESIAN_POINT('Ctrl Pts',(33.6743371481683,38.7500000136559,-33.6743371481684));
#6551=CARTESIAN_POINT('Ctrl Pts',(39.8371685740842,38.5416666803226,-23.));
#6552=CARTESIAN_POINT('Ctrl Pts',(46.,38.3333333469893,-12.3256628518317));
#6553=CARTESIAN_POINT('Ctrl Pts',(46.,38.1250000136559,-5.63337527607782E-15));
#6554=CARTESIAN_POINT('Ctrl Pts',(46.,37.9166666803226,12.3256628518316));
#6555=CARTESIAN_POINT('Ctrl Pts',(39.8371685740842,37.7083333469893,23.));
#6556=CARTESIAN_POINT('Ctrl Pts',(33.6743371481684,37.5000000136559,33.6743371481683));
#6557=CARTESIAN_POINT('Ctrl Pts',(23.,37.2916666803226,39.8371685740842));
#6558=CARTESIAN_POINT('Ctrl Pts',(12.3256628518317,37.0833333469893,46.));
#6559=CARTESIAN_POINT('Ctrl Pts',(8.45006291411674E-15,36.8750000136559,
46.));
#6560=CARTESIAN_POINT('Ctrl Pts',(-12.3256628518316,36.6666666803226,46.));
#6561=CARTESIAN_POINT('Ctrl Pts',(-23.,36.4583333469893,39.8371685740842));
#6562=CARTESIAN_POINT('Ctrl Pts',(-33.6743371481683,36.2500000136559,33.6743371481684));
#6563=CARTESIAN_POINT('Ctrl Pts',(-39.8371685740842,36.0416666803226,23.));
#6564=CARTESIAN_POINT('Ctrl Pts',(-46.,35.8333333469893,12.3256628518317));
#6565=CARTESIAN_POINT('Ctrl Pts',(-46.,35.6250000136559,0.));
#6566=CARTESIAN_POINT('Ctrl Pts',(-46.,35.4166666803226,-12.3256628518316));
#6567=CARTESIAN_POINT('Ctrl Pts',(-39.8371685740842,35.2083333469893,-23.));
#6568=CARTESIAN_POINT('Ctrl Pts',(-33.6743371481684,35.0000000136559,-33.6743371481684));
#6569=CARTESIAN_POINT('Ctrl Pts',(-23.,34.7916666803226,-39.8371685740842));
#6570=CARTESIAN_POINT('Ctrl Pts',(-12.3256628518317,34.5833333469893,-46.));
#6571=CARTESIAN_POINT('Ctrl Pts',(-2.81668763803891E-15,34.3750000136559,
-46.));
#6572=CARTESIAN_POINT('Ctrl Pts',(12.3256628518316,34.1666666803226,-46.));
#6573=CARTESIAN_POINT('Ctrl Pts',(23.,33.9583333469893,-39.8371685740842));
#6574=CARTESIAN_POINT('Ctrl Pts',(33.6743371481683,33.7500000136559,-33.6743371481684));
#6575=CARTESIAN_POINT('Ctrl Pts',(39.8371685740842,33.5416666803226,-23.));
#6576=CARTESIAN_POINT('Ctrl Pts',(46.,33.3333333469893,-12.3256628518317));
#6577=CARTESIAN_POINT('Ctrl Pts',(46.,33.1250000136559,-5.63337527607782E-15));
#6578=CARTESIAN_POINT('Ctrl Pts',(46.,32.9166666803226,12.3256628518316));
#6579=CARTESIAN_POINT('Ctrl Pts',(39.8371685740842,32.7083333469893,23.));
#6580=CARTESIAN_POINT('Ctrl Pts',(33.6743371481684,32.5000000136559,33.6743371481683));
#6581=CARTESIAN_POINT('Ctrl Pts',(23.,32.2916666803226,39.8371685740842));
#6582=CARTESIAN_POINT('Ctrl Pts',(12.3256628518317,32.0833333469893,46.));
#6583=CARTESIAN_POINT('Ctrl Pts',(8.45006291411674E-15,31.8750000136559,
46.));
#6584=CARTESIAN_POINT('Ctrl Pts',(-12.3256628518316,31.6666666803226,46.));
#6585=CARTESIAN_POINT('Ctrl Pts',(-23.,31.4583333469893,39.8371685740842));
#6586=CARTESIAN_POINT('Ctrl Pts',(-33.6743371481683,31.2500000136559,33.6743371481684));
#6587=CARTESIAN_POINT('Ctrl Pts',(-39.8371685740842,31.0416666803226,23.));
#6588=CARTESIAN_POINT('Ctrl Pts',(-46.,30.8333333469893,12.3256628518317));
#6589=CARTESIAN_POINT('Ctrl Pts',(-46.,30.6250000136559,0.));
#6590=CARTESIAN_POINT('Ctrl Pts',(-46.,30.4166666803226,-12.3256628518316));
#6591=CARTESIAN_POINT('Ctrl Pts',(-39.8371685740842,30.2083333469893,-23.));
#6592=CARTESIAN_POINT('Ctrl Pts',(-33.6743371481684,30.0000000136559,-33.6743371481684));
#6593=CARTESIAN_POINT('Ctrl Pts',(-23.,29.7916666803226,-39.8371685740842));
#6594=CARTESIAN_POINT('Ctrl Pts',(-12.3256628518317,29.5833333469893,-46.));
#6595=CARTESIAN_POINT('Ctrl Pts',(-2.81668763803891E-15,29.3750000136559,
-46.));
#6596=CARTESIAN_POINT('Ctrl Pts',(12.3256628518316,29.1666666803226,-46.));
#6597=CARTESIAN_POINT('Ctrl Pts',(23.,28.9583333469893,-39.8371685740842));
#6598=CARTESIAN_POINT('Ctrl Pts',(33.6743371481683,28.7500000136559,-33.6743371481684));
#6599=CARTESIAN_POINT('Ctrl Pts',(39.8371685740842,28.5416666803226,-23.));
#6600=CARTESIAN_POINT('Ctrl Pts',(46.,28.3333333469893,-12.3256628518317));
#6601=CARTESIAN_POINT('Ctrl Pts',(46.,28.1250000136559,-5.63337527607782E-15));
#6602=CARTESIAN_POINT('Ctrl Pts',(46.,27.9166666803226,12.3256628518316));
#6603=CARTESIAN_POINT('Ctrl Pts',(39.8371685740842,27.7083333469893,23.));
#6604=CARTESIAN_POINT('Ctrl Pts',(33.6743371481684,27.5000000136559,33.6743371481683));
#6605=CARTESIAN_POINT('Ctrl Pts',(23.,27.2916666803226,39.8371685740842));
#6606=CARTESIAN_POINT('Ctrl Pts',(12.3256628518317,27.0833333469893,46.));
#6607=CARTESIAN_POINT('Ctrl Pts',(8.45006291411674E-15,26.8750000136559,
46.));
#6608=CARTESIAN_POINT('Ctrl Pts',(-12.3256628518316,26.6666666803226,46.));
#6609=CARTESIAN_POINT('Ctrl Pts',(-23.,26.4583333469893,39.8371685740842));
#6610=CARTESIAN_POINT('Ctrl Pts',(-33.6743371481683,26.2500000136559,33.6743371481684));
#6611=CARTESIAN_POINT('Ctrl Pts',(-39.8371685740842,26.0416666803226,23.));
#6612=CARTESIAN_POINT('Ctrl Pts',(-46.,25.8333333469893,12.3256628518317));
#6613=CARTESIAN_POINT('Ctrl Pts',(-46.,25.6250000136559,0.));
#6614=CARTESIAN_POINT('Ctrl Pts',(-48.706329375,57.187500006828,-1.8898197019151E-14));
#6615=CARTESIAN_POINT('Ctrl Pts',(-48.706329375,56.9791666734946,-13.0508216223155));
#6616=CARTESIAN_POINT('Ctrl Pts',(-42.1809185638422,56.7708333401613,-24.3531646875));
#6617=CARTESIAN_POINT('Ctrl Pts',(-35.6555077526845,56.562500006828,-35.6555077526845));
#6618=CARTESIAN_POINT('Ctrl Pts',(-24.3531646875,56.3541666734946,-42.1809185638423));
#6619=CARTESIAN_POINT('Ctrl Pts',(-13.0508216223155,56.1458333401613,-48.706329375));
#6620=CARTESIAN_POINT('Ctrl Pts',(1.59157945007855E-14,55.937500006828,
-48.706329375));
#6621=CARTESIAN_POINT('Ctrl Pts',(13.0508216223155,55.7291666734946,-48.706329375));
#6622=CARTESIAN_POINT('Ctrl Pts',(24.3531646875,55.5208333401613,-42.1809185638422));
#6623=CARTESIAN_POINT('Ctrl Pts',(35.6555077526845,55.312500006828,-35.6555077526845));
#6624=CARTESIAN_POINT('Ctrl Pts',(42.1809185638422,55.1041666734946,-24.3531646875));
#6625=CARTESIAN_POINT('Ctrl Pts',(48.706329375,54.8958333401613,-13.0508216223155));
#6626=CARTESIAN_POINT('Ctrl Pts',(48.706329375,54.687500006828,1.293339198242E-14));
#6627=CARTESIAN_POINT('Ctrl Pts',(48.706329375,54.4791666734946,13.0508216223155));
#6628=CARTESIAN_POINT('Ctrl Pts',(42.1809185638422,54.2708333401613,24.3531646875));
#6629=CARTESIAN_POINT('Ctrl Pts',(35.6555077526845,54.062500006828,35.6555077526845));
#6630=CARTESIAN_POINT('Ctrl Pts',(24.3531646875,53.8541666734946,42.1809185638422));
#6631=CARTESIAN_POINT('Ctrl Pts',(13.0508216223155,53.6458333401613,48.706329375));
#6632=CARTESIAN_POINT('Ctrl Pts',(-9.95098946405443E-15,53.437500006828,
48.706329375));
#6633=CARTESIAN_POINT('Ctrl Pts',(-13.0508216223155,53.2291666734946,48.706329375));
#6634=CARTESIAN_POINT('Ctrl Pts',(-24.3531646875,53.0208333401613,42.1809185638423));
#6635=CARTESIAN_POINT('Ctrl Pts',(-35.6555077526845,52.812500006828,35.6555077526845));
#6636=CARTESIAN_POINT('Ctrl Pts',(-42.1809185638422,52.6041666734946,24.3531646875));
#6637=CARTESIAN_POINT('Ctrl Pts',(-48.706329375,52.3958333401613,13.0508216223155));
#6638=CARTESIAN_POINT('Ctrl Pts',(-48.706329375,52.187500006828,-1.8898197019151E-14));
#6639=CARTESIAN_POINT('Ctrl Pts',(-48.706329375,51.9791666734946,-13.0508216223155));
#6640=CARTESIAN_POINT('Ctrl Pts',(-42.1809185638422,51.7708333401613,-24.3531646875));
#6641=CARTESIAN_POINT('Ctrl Pts',(-35.6555077526845,51.562500006828,-35.6555077526845));
#6642=CARTESIAN_POINT('Ctrl Pts',(-24.3531646875,51.3541666734946,-42.1809185638423));
#6643=CARTESIAN_POINT('Ctrl Pts',(-13.0508216223155,51.1458333401613,-48.706329375));
#6644=CARTESIAN_POINT('Ctrl Pts',(1.59157945007855E-14,50.937500006828,
-48.706329375));
#6645=CARTESIAN_POINT('Ctrl Pts',(13.0508216223155,50.7291666734946,-48.706329375));
#6646=CARTESIAN_POINT('Ctrl Pts',(24.3531646875,50.5208333401613,-42.1809185638422));
#6647=CARTESIAN_POINT('Ctrl Pts',(35.6555077526845,50.312500006828,-35.6555077526845));
#6648=CARTESIAN_POINT('Ctrl Pts',(42.1809185638422,50.1041666734946,-24.3531646875));
#6649=CARTESIAN_POINT('Ctrl Pts',(48.706329375,49.8958333401613,-13.0508216223155));
#6650=CARTESIAN_POINT('Ctrl Pts',(48.706329375,49.687500006828,1.293339198242E-14));
#6651=CARTESIAN_POINT('Ctrl Pts',(48.706329375,49.4791666734946,13.0508216223155));
#6652=CARTESIAN_POINT('Ctrl Pts',(42.1809185638422,49.2708333401613,24.3531646875));
#6653=CARTESIAN_POINT('Ctrl Pts',(35.6555077526845,49.062500006828,35.6555077526845));
#6654=CARTESIAN_POINT('Ctrl Pts',(24.3531646875,48.8541666734946,42.1809185638422));
#6655=CARTESIAN_POINT('Ctrl Pts',(13.0508216223155,48.6458333401613,48.706329375));
#6656=CARTESIAN_POINT('Ctrl Pts',(-9.95098946405443E-15,48.437500006828,
48.706329375));
#6657=CARTESIAN_POINT('Ctrl Pts',(-13.0508216223155,48.2291666734946,48.706329375));
#6658=CARTESIAN_POINT('Ctrl Pts',(-24.3531646875,48.0208333401613,42.1809185638423));
#6659=CARTESIAN_POINT('Ctrl Pts',(-35.6555077526845,47.812500006828,35.6555077526845));
#6660=CARTESIAN_POINT('Ctrl Pts',(-42.1809185638422,47.6041666734946,24.3531646875));
#6661=CARTESIAN_POINT('Ctrl Pts',(-48.706329375,47.3958333401613,13.0508216223155));
#6662=CARTESIAN_POINT('Ctrl Pts',(-48.706329375,47.187500006828,-1.8898197019151E-14));
#6663=CARTESIAN_POINT('Ctrl Pts',(-48.706329375,46.9791666734946,-13.0508216223155));
#6664=CARTESIAN_POINT('Ctrl Pts',(-42.1809185638422,46.7708333401613,-24.3531646875));
#6665=CARTESIAN_POINT('Ctrl Pts',(-35.6555077526845,46.562500006828,-35.6555077526845));
#6666=CARTESIAN_POINT('Ctrl Pts',(-24.3531646875,46.3541666734946,-42.1809185638423));
#6667=CARTESIAN_POINT('Ctrl Pts',(-13.0508216223155,46.1458333401613,-48.706329375));
#6668=CARTESIAN_POINT('Ctrl Pts',(1.59157945007855E-14,45.937500006828,
-48.706329375));
#6669=CARTESIAN_POINT('Ctrl Pts',(13.0508216223155,45.7291666734946,-48.706329375));
#6670=CARTESIAN_POINT('Ctrl Pts',(24.3531646875,45.5208333401613,-42.1809185638422));
#6671=CARTESIAN_POINT('Ctrl Pts',(35.6555077526845,45.312500006828,-35.6555077526845));
#6672=CARTESIAN_POINT('Ctrl Pts',(42.1809185638422,45.1041666734946,-24.3531646875));
#6673=CARTESIAN_POINT('Ctrl Pts',(48.706329375,44.8958333401613,-13.0508216223155));
#6674=CARTESIAN_POINT('Ctrl Pts',(48.706329375,44.687500006828,1.293339198242E-14));
#6675=CARTESIAN_POINT('Ctrl Pts',(48.706329375,44.4791666734946,13.0508216223155));
#6676=CARTESIAN_POINT('Ctrl Pts',(42.1809185638422,44.2708333401613,24.3531646875));
#6677=CARTESIAN_POINT('Ctrl Pts',(35.6555077526845,44.062500006828,35.6555077526845));
#6678=CARTESIAN_POINT('Ctrl Pts',(24.3531646875,43.8541666734946,42.1809185638422));
#6679=CARTESIAN_POINT('Ctrl Pts',(13.0508216223155,43.6458333401613,48.706329375));
#6680=CARTESIAN_POINT('Ctrl Pts',(-9.95098946405443E-15,43.437500006828,
48.706329375));
#6681=CARTESIAN_POINT('Ctrl Pts',(-13.0508216223155,43.2291666734946,48.706329375));
#6682=CARTESIAN_POINT('Ctrl Pts',(-24.3531646875,43.0208333401613,42.1809185638423));
#6683=CARTESIAN_POINT('Ctrl Pts',(-35.6555077526845,42.812500006828,35.6555077526845));
#6684=CARTESIAN_POINT('Ctrl Pts',(-42.1809185638422,42.6041666734946,24.3531646875));
#6685=CARTESIAN_POINT('Ctrl Pts',(-48.706329375,42.3958333401613,13.0508216223155));
#6686=CARTESIAN_POINT('Ctrl Pts',(-48.706329375,42.187500006828,-1.8898197019151E-14));
#6687=CARTESIAN_POINT('Ctrl Pts',(-48.706329375,41.9791666734946,-13.0508216223155));
#6688=CARTESIAN_POINT('Ctrl Pts',(-42.1809185638422,41.7708333401613,-24.3531646875));
#6689=CARTESIAN_POINT('Ctrl Pts',(-35.6555077526845,41.562500006828,-35.6555077526845));
#6690=CARTESIAN_POINT('Ctrl Pts',(-24.3531646875,41.3541666734946,-42.1809185638423));
#6691=CARTESIAN_POINT('Ctrl Pts',(-13.0508216223155,41.1458333401613,-48.706329375));
#6692=CARTESIAN_POINT('Ctrl Pts',(1.59157945007855E-14,40.937500006828,
-48.706329375));
#6693=CARTESIAN_POINT('Ctrl Pts',(13.0508216223155,40.7291666734946,-48.706329375));
#6694=CARTESIAN_POINT('Ctrl Pts',(24.3531646875,40.5208333401613,-42.1809185638422));
#6695=CARTESIAN_POINT('Ctrl Pts',(35.6555077526845,40.312500006828,-35.6555077526845));
#6696=CARTESIAN_POINT('Ctrl Pts',(42.1809185638422,40.1041666734946,-24.3531646875));
#6697=CARTESIAN_POINT('Ctrl Pts',(48.706329375,39.8958333401613,-13.0508216223155));
#6698=CARTESIAN_POINT('Ctrl Pts',(48.706329375,39.687500006828,1.293339198242E-14));
#6699=CARTESIAN_POINT('Ctrl Pts',(48.706329375,39.4791666734946,13.0508216223155));
#6700=CARTESIAN_POINT('Ctrl Pts',(42.1809185638422,39.2708333401613,24.3531646875));
#6701=CARTESIAN_POINT('Ctrl Pts',(35.6555077526845,39.062500006828,35.6555077526845));
#6702=CARTESIAN_POINT('Ctrl Pts',(24.3531646875,38.8541666734946,42.1809185638422));
#6703=CARTESIAN_POINT('Ctrl Pts',(13.0508216223155,38.6458333401613,48.706329375));
#6704=CARTESIAN_POINT('Ctrl Pts',(-9.95098946405443E-15,38.437500006828,
48.706329375));
#6705=CARTESIAN_POINT('Ctrl Pts',(-13.0508216223155,38.2291666734946,48.706329375));
#6706=CARTESIAN_POINT('Ctrl Pts',(-24.3531646875,38.0208333401613,42.1809185638423));
#6707=CARTESIAN_POINT('Ctrl Pts',(-35.6555077526845,37.812500006828,35.6555077526845));
#6708=CARTESIAN_POINT('Ctrl Pts',(-42.1809185638422,37.6041666734946,24.3531646875));
#6709=CARTESIAN_POINT('Ctrl Pts',(-48.706329375,37.3958333401613,13.0508216223155));
#6710=CARTESIAN_POINT('Ctrl Pts',(-48.706329375,37.187500006828,-1.8898197019151E-14));
#6711=CARTESIAN_POINT('Ctrl Pts',(-48.706329375,36.9791666734946,-13.0508216223155));
#6712=CARTESIAN_POINT('Ctrl Pts',(-42.1809185638422,36.7708333401613,-24.3531646875));
#6713=CARTESIAN_POINT('Ctrl Pts',(-35.6555077526845,36.562500006828,-35.6555077526845));
#6714=CARTESIAN_POINT('Ctrl Pts',(-24.3531646875,36.3541666734946,-42.1809185638423));
#6715=CARTESIAN_POINT('Ctrl Pts',(-13.0508216223155,36.1458333401613,-48.706329375));
#6716=CARTESIAN_POINT('Ctrl Pts',(1.59157945007855E-14,35.937500006828,
-48.706329375));
#6717=CARTESIAN_POINT('Ctrl Pts',(13.0508216223155,35.7291666734946,-48.706329375));
#6718=CARTESIAN_POINT('Ctrl Pts',(24.3531646875,35.5208333401613,-42.1809185638422));
#6719=CARTESIAN_POINT('Ctrl Pts',(35.6555077526845,35.312500006828,-35.6555077526845));
#6720=CARTESIAN_POINT('Ctrl Pts',(42.1809185638422,35.1041666734946,-24.3531646875));
#6721=CARTESIAN_POINT('Ctrl Pts',(48.706329375,34.8958333401613,-13.0508216223155));
#6722=CARTESIAN_POINT('Ctrl Pts',(48.706329375,34.687500006828,1.293339198242E-14));
#6723=CARTESIAN_POINT('Ctrl Pts',(48.706329375,34.4791666734946,13.0508216223155));
#6724=CARTESIAN_POINT('Ctrl Pts',(42.1809185638422,34.2708333401613,24.3531646875));
#6725=CARTESIAN_POINT('Ctrl Pts',(35.6555077526845,34.062500006828,35.6555077526845));
#6726=CARTESIAN_POINT('Ctrl Pts',(24.3531646875,33.8541666734946,42.1809185638422));
#6727=CARTESIAN_POINT('Ctrl Pts',(13.0508216223155,33.6458333401613,48.706329375));
#6728=CARTESIAN_POINT('Ctrl Pts',(-9.95098946405443E-15,33.437500006828,
48.706329375));
#6729=CARTESIAN_POINT('Ctrl Pts',(-13.0508216223155,33.2291666734946,48.706329375));
#6730=CARTESIAN_POINT('Ctrl Pts',(-24.3531646875,33.0208333401613,42.1809185638423));
#6731=CARTESIAN_POINT('Ctrl Pts',(-35.6555077526845,32.812500006828,35.6555077526845));
#6732=CARTESIAN_POINT('Ctrl Pts',(-42.1809185638422,32.6041666734946,24.3531646875));
#6733=CARTESIAN_POINT('Ctrl Pts',(-48.706329375,32.3958333401613,13.0508216223155));
#6734=CARTESIAN_POINT('Ctrl Pts',(-48.706329375,32.187500006828,-1.8898197019151E-14));
#6735=CARTESIAN_POINT('Ctrl Pts',(-48.706329375,31.9791666734946,-13.0508216223155));
#6736=CARTESIAN_POINT('Ctrl Pts',(-42.1809185638422,31.7708333401613,-24.3531646875));
#6737=CARTESIAN_POINT('Ctrl Pts',(-35.6555077526845,31.562500006828,-35.6555077526845));
#6738=CARTESIAN_POINT('Ctrl Pts',(-24.3531646875,31.3541666734946,-42.1809185638423));
#6739=CARTESIAN_POINT('Ctrl Pts',(-13.0508216223155,31.1458333401613,-48.706329375));
#6740=CARTESIAN_POINT('Ctrl Pts',(1.59157945007855E-14,30.937500006828,
-48.706329375));
#6741=CARTESIAN_POINT('Ctrl Pts',(13.0508216223155,30.7291666734946,-48.706329375));
#6742=CARTESIAN_POINT('Ctrl Pts',(24.3531646875,30.5208333401613,-42.1809185638422));
#6743=CARTESIAN_POINT('Ctrl Pts',(35.6555077526845,30.312500006828,-35.6555077526845));
#6744=CARTESIAN_POINT('Ctrl Pts',(42.1809185638422,30.1041666734946,-24.3531646875));
#6745=CARTESIAN_POINT('Ctrl Pts',(48.706329375,29.8958333401613,-13.0508216223155));
#6746=CARTESIAN_POINT('Ctrl Pts',(48.706329375,29.687500006828,1.293339198242E-14));
#6747=CARTESIAN_POINT('Ctrl Pts',(48.706329375,29.4791666734946,13.0508216223155));
#6748=CARTESIAN_POINT('Ctrl Pts',(42.1809185638422,29.2708333401613,24.3531646875));
#6749=CARTESIAN_POINT('Ctrl Pts',(35.6555077526845,29.062500006828,35.6555077526845));
#6750=CARTESIAN_POINT('Ctrl Pts',(24.3531646875,28.8541666734946,42.1809185638422));
#6751=CARTESIAN_POINT('Ctrl Pts',(13.0508216223155,28.6458333401613,48.706329375));
#6752=CARTESIAN_POINT('Ctrl Pts',(-9.95098946405443E-15,28.437500006828,
48.706329375));
#6753=CARTESIAN_POINT('Ctrl Pts',(-13.0508216223155,28.2291666734946,48.706329375));
#6754=CARTESIAN_POINT('Ctrl Pts',(-24.3531646875,28.0208333401613,42.1809185638423));
#6755=CARTESIAN_POINT('Ctrl Pts',(-35.6555077526845,27.812500006828,35.6555077526845));
#6756=CARTESIAN_POINT('Ctrl Pts',(-42.1809185638422,27.6041666734946,24.3531646875));
#6757=CARTESIAN_POINT('Ctrl Pts',(-48.706329375,27.3958333401613,13.0508216223155));
#6758=CARTESIAN_POINT('Ctrl Pts',(-48.706329375,27.187500006828,-1.8898197019151E-14));
#6759=CARTESIAN_POINT('',(48.5725845633798,49.6293483229262,3.60701400320328));
#6760=CARTESIAN_POINT('Ctrl Pts',(45.858362923034,48.0633913333999,3.60701400320327));
#6761=CARTESIAN_POINT('Ctrl Pts',(46.089925771934,48.1969849680263,3.60701400320324));
#6762=CARTESIAN_POINT('Ctrl Pts',(46.5530501979845,48.4641744416604,3.60701400320326));
#6763=CARTESIAN_POINT('Ctrl Pts',(47.0161721905706,48.7313681332063,3.60701400320324));
#6764=CARTESIAN_POINT('Ctrl Pts',(47.6893519862319,49.1197565257476,3.60701400320324));
#6765=CARTESIAN_POINT('Ctrl Pts',(48.1309692507095,49.3745507329179,3.60701400320328));
#6766=CARTESIAN_POINT('Ctrl Pts',(48.5725845633798,49.6293483229262,3.60701400320328));
#6767=CARTESIAN_POINT('',(3.61292728433797,48.4957479656467,48.5721450795008));
#6768=CARTESIAN_POINT('Ctrl Pts',(48.5725845633798,49.6293483229262,3.60701400320328));
#6769=CARTESIAN_POINT('Ctrl Pts',(47.7480251419552,49.4485714020251,14.7106532430575));
#6770=CARTESIAN_POINT('Ctrl Pts',(42.1809185638422,49.2708333401613,24.3531646875));
#6771=CARTESIAN_POINT('Ctrl Pts',(35.6555077526845,49.062500006828,35.6555077526845));
#6772=CARTESIAN_POINT('Ctrl Pts',(24.3531646875,48.8541666734946,42.1809185638422));
#6773=CARTESIAN_POINT('Ctrl Pts',(14.7133549689477,48.6764784118853,47.7464652997852));
#6774=CARTESIAN_POINT('Ctrl Pts',(3.61292728433797,48.4957479656467,48.5721450795008));
#6775=CARTESIAN_POINT('Ctrl Pts',(3.61292728433797,48.4957479656467,48.5721450795008));
#6776=CARTESIAN_POINT('Ctrl Pts',(3.61292728433797,48.3625660950884,48.3403451622817));
#6777=CARTESIAN_POINT('Ctrl Pts',(3.612927284338,48.2293911846469,48.1085412459393));
#6778=CARTESIAN_POINT('Ctrl Pts',(3.612927284338,47.9630558994543,47.6449250631479));
#6779=CARTESIAN_POINT('Ctrl Pts',(3.61292728433804,47.8298955244832,47.4131127965212));
#6780=CARTESIAN_POINT('Ctrl Pts',(3.61292728433804,47.6967427432646,47.1812961682826));
#6781=CARTESIAN_POINT('Ctrl Pts',(3.61292728433804,47.4433704509922,46.7401795055578));
#6782=CARTESIAN_POINT('Ctrl Pts',(3.61292728433798,47.1900256371662,46.2990470581854));
#6783=CARTESIAN_POINT('Ctrl Pts',(3.61292728433798,46.936710750803,45.8578974271399));
#6784=CARTESIAN_POINT('Ctrl Pts',(-46.,55.6250000136559,0.));
#6785=CARTESIAN_POINT('Ctrl Pts',(-46.,55.4166666803226,-12.3256628518316));
#6786=CARTESIAN_POINT('Ctrl Pts',(-39.8371685740842,55.2083333469893,-23.));
#6787=CARTESIAN_POINT('Ctrl Pts',(-33.6743371481684,55.0000000136559,-33.6743371481684));
#6788=CARTESIAN_POINT('Ctrl Pts',(-23.,54.7916666803226,-39.8371685740842));
#6789=CARTESIAN_POINT('Ctrl Pts',(-12.3256628518317,54.5833333469893,-46.));
#6790=CARTESIAN_POINT('Ctrl Pts',(-2.81668763803891E-15,54.3750000136559,
-46.));
#6791=CARTESIAN_POINT('Ctrl Pts',(12.3256628518316,54.1666666803226,-46.));
#6792=CARTESIAN_POINT('Ctrl Pts',(23.,53.9583333469893,-39.8371685740842));
#6793=CARTESIAN_POINT('Ctrl Pts',(33.6743371481683,53.7500000136559,-33.6743371481684));
#6794=CARTESIAN_POINT('Ctrl Pts',(39.8371685740842,53.5416666803226,-23.));
#6795=CARTESIAN_POINT('Ctrl Pts',(46.,53.3333333469893,-12.3256628518317));
#6796=CARTESIAN_POINT('Ctrl Pts',(46.,53.1250000136559,-5.63337527607782E-15));
#6797=CARTESIAN_POINT('Ctrl Pts',(46.,52.9166666803226,12.3256628518316));
#6798=CARTESIAN_POINT('Ctrl Pts',(39.8371685740842,52.7083333469893,23.));
#6799=CARTESIAN_POINT('Ctrl Pts',(33.6743371481684,52.5000000136559,33.6743371481683));
#6800=CARTESIAN_POINT('Ctrl Pts',(23.,52.2916666803226,39.8371685740842));
#6801=CARTESIAN_POINT('Ctrl Pts',(12.3256628518317,52.0833333469893,46.));
#6802=CARTESIAN_POINT('Ctrl Pts',(8.45006291411674E-15,51.8750000136559,
46.));
#6803=CARTESIAN_POINT('Ctrl Pts',(-12.3256628518316,51.6666666803226,46.));
#6804=CARTESIAN_POINT('Ctrl Pts',(-23.,51.4583333469893,39.8371685740842));
#6805=CARTESIAN_POINT('Ctrl Pts',(-33.6743371481683,51.2500000136559,33.6743371481684));
#6806=CARTESIAN_POINT('Ctrl Pts',(-39.8371685740842,51.0416666803226,23.));
#6807=CARTESIAN_POINT('Ctrl Pts',(-46.,50.8333333469893,12.3256628518317));
#6808=CARTESIAN_POINT('Ctrl Pts',(-46.,50.6250000136559,0.));
#6809=CARTESIAN_POINT('Ctrl Pts',(-46.,50.4166666803226,-12.3256628518316));
#6810=CARTESIAN_POINT('Ctrl Pts',(-39.8371685740842,50.2083333469893,-23.));
#6811=CARTESIAN_POINT('Ctrl Pts',(-33.6743371481684,50.0000000136559,-33.6743371481684));
#6812=CARTESIAN_POINT('Ctrl Pts',(-23.,49.7916666803226,-39.8371685740842));
#6813=CARTESIAN_POINT('Ctrl Pts',(-12.3256628518317,49.5833333469893,-46.));
#6814=CARTESIAN_POINT('Ctrl Pts',(-2.81668763803891E-15,49.3750000136559,
-46.));
#6815=CARTESIAN_POINT('Ctrl Pts',(12.3256628518316,49.1666666803226,-46.));
#6816=CARTESIAN_POINT('Ctrl Pts',(23.,48.9583333469893,-39.8371685740842));
#6817=CARTESIAN_POINT('Ctrl Pts',(33.6743371481683,48.7500000136559,-33.6743371481684));
#6818=CARTESIAN_POINT('Ctrl Pts',(39.8371685740842,48.5416666803226,-23.));
#6819=CARTESIAN_POINT('Ctrl Pts',(46.,48.3333333469893,-12.3256628518317));
#6820=CARTESIAN_POINT('Ctrl Pts',(46.,48.1250000136559,-5.63337527607782E-15));
#6821=CARTESIAN_POINT('Ctrl Pts',(46.,47.9166666803226,12.3256628518316));
#6822=CARTESIAN_POINT('Ctrl Pts',(39.8371685740842,47.7083333469893,23.));
#6823=CARTESIAN_POINT('Ctrl Pts',(33.6743371481684,47.5000000136559,33.6743371481683));
#6824=CARTESIAN_POINT('Ctrl Pts',(23.,47.2916666803226,39.8371685740842));
#6825=CARTESIAN_POINT('Ctrl Pts',(12.3256628518317,47.0833333469893,46.));
#6826=CARTESIAN_POINT('Ctrl Pts',(8.45006291411674E-15,46.8750000136559,
46.));
#6827=CARTESIAN_POINT('Ctrl Pts',(-12.3256628518316,46.6666666803226,46.));
#6828=CARTESIAN_POINT('Ctrl Pts',(-23.,46.4583333469893,39.8371685740842));
#6829=CARTESIAN_POINT('Ctrl Pts',(-33.6743371481683,46.2500000136559,33.6743371481684));
#6830=CARTESIAN_POINT('Ctrl Pts',(-39.8371685740842,46.0416666803226,23.));
#6831=CARTESIAN_POINT('Ctrl Pts',(-46.,45.8333333469892,12.3256628518317));
#6832=CARTESIAN_POINT('Ctrl Pts',(-46.,45.6250000136559,0.));
#6833=CARTESIAN_POINT('Ctrl Pts',(-46.,45.4166666803226,-12.3256628518316));
#6834=CARTESIAN_POINT('Ctrl Pts',(-39.8371685740842,45.2083333469893,-23.));
#6835=CARTESIAN_POINT('Ctrl Pts',(-33.6743371481684,45.0000000136559,-33.6743371481684));
#6836=CARTESIAN_POINT('Ctrl Pts',(-23.,44.7916666803226,-39.8371685740842));
#6837=CARTESIAN_POINT('Ctrl Pts',(-12.3256628518317,44.5833333469893,-46.));
#6838=CARTESIAN_POINT('Ctrl Pts',(-2.81668763803891E-15,44.3750000136559,
-46.));
#6839=CARTESIAN_POINT('Ctrl Pts',(12.3256628518316,44.1666666803226,-46.));
#6840=CARTESIAN_POINT('Ctrl Pts',(23.,43.9583333469893,-39.8371685740842));
#6841=CARTESIAN_POINT('Ctrl Pts',(33.6743371481683,43.7500000136559,-33.6743371481684));
#6842=CARTESIAN_POINT('Ctrl Pts',(39.8371685740842,43.5416666803226,-23.));
#6843=CARTESIAN_POINT('Ctrl Pts',(46.,43.3333333469893,-12.3256628518317));
#6844=CARTESIAN_POINT('Ctrl Pts',(46.,43.1250000136559,-5.63337527607782E-15));
#6845=CARTESIAN_POINT('Ctrl Pts',(46.,42.9166666803226,12.3256628518316));
#6846=CARTESIAN_POINT('Ctrl Pts',(39.8371685740842,42.7083333469893,23.));
#6847=CARTESIAN_POINT('Ctrl Pts',(33.6743371481684,42.5000000136559,33.6743371481683));
#6848=CARTESIAN_POINT('Ctrl Pts',(23.,42.2916666803226,39.8371685740842));
#6849=CARTESIAN_POINT('Ctrl Pts',(12.3256628518317,42.0833333469893,46.));
#6850=CARTESIAN_POINT('Ctrl Pts',(8.45006291411674E-15,41.8750000136559,
46.));
#6851=CARTESIAN_POINT('Ctrl Pts',(-12.3256628518316,41.6666666803226,46.));
#6852=CARTESIAN_POINT('Ctrl Pts',(-23.,41.4583333469893,39.8371685740842));
#6853=CARTESIAN_POINT('Ctrl Pts',(-33.6743371481683,41.2500000136559,33.6743371481684));
#6854=CARTESIAN_POINT('Ctrl Pts',(-39.8371685740842,41.0416666803226,23.));
#6855=CARTESIAN_POINT('Ctrl Pts',(-46.,40.8333333469893,12.3256628518317));
#6856=CARTESIAN_POINT('Ctrl Pts',(-46.,40.6250000136559,0.));
#6857=CARTESIAN_POINT('Ctrl Pts',(-46.,40.4166666803226,-12.3256628518316));
#6858=CARTESIAN_POINT('Ctrl Pts',(-39.8371685740842,40.2083333469893,-23.));
#6859=CARTESIAN_POINT('Ctrl Pts',(-33.6743371481684,40.0000000136559,-33.6743371481684));
#6860=CARTESIAN_POINT('Ctrl Pts',(-23.,39.7916666803226,-39.8371685740842));
#6861=CARTESIAN_POINT('Ctrl Pts',(-12.3256628518317,39.5833333469893,-46.));
#6862=CARTESIAN_POINT('Ctrl Pts',(-2.81668763803891E-15,39.3750000136559,
-46.));
#6863=CARTESIAN_POINT('Ctrl Pts',(12.3256628518316,39.1666666803226,-46.));
#6864=CARTESIAN_POINT('Ctrl Pts',(23.,38.9583333469893,-39.8371685740842));
#6865=CARTESIAN_POINT('Ctrl Pts',(33.6743371481683,38.7500000136559,-33.6743371481684));
#6866=CARTESIAN_POINT('Ctrl Pts',(39.8371685740842,38.5416666803226,-23.));
#6867=CARTESIAN_POINT('Ctrl Pts',(46.,38.3333333469893,-12.3256628518317));
#6868=CARTESIAN_POINT('Ctrl Pts',(46.,38.1250000136559,-5.63337527607782E-15));
#6869=CARTESIAN_POINT('Ctrl Pts',(46.,37.9166666803226,12.3256628518316));
#6870=CARTESIAN_POINT('Ctrl Pts',(39.8371685740842,37.7083333469893,23.));
#6871=CARTESIAN_POINT('Ctrl Pts',(33.6743371481684,37.5000000136559,33.6743371481683));
#6872=CARTESIAN_POINT('Ctrl Pts',(23.,37.2916666803226,39.8371685740842));
#6873=CARTESIAN_POINT('Ctrl Pts',(12.3256628518317,37.0833333469893,46.));
#6874=CARTESIAN_POINT('Ctrl Pts',(8.45006291411674E-15,36.8750000136559,
46.));
#6875=CARTESIAN_POINT('Ctrl Pts',(-12.3256628518316,36.6666666803226,46.));
#6876=CARTESIAN_POINT('Ctrl Pts',(-23.,36.4583333469893,39.8371685740842));
#6877=CARTESIAN_POINT('Ctrl Pts',(-33.6743371481683,36.2500000136559,33.6743371481684));
#6878=CARTESIAN_POINT('Ctrl Pts',(-39.8371685740842,36.0416666803226,23.));
#6879=CARTESIAN_POINT('Ctrl Pts',(-46.,35.8333333469893,12.3256628518317));
#6880=CARTESIAN_POINT('Ctrl Pts',(-46.,35.6250000136559,0.));
#6881=CARTESIAN_POINT('Ctrl Pts',(-46.,35.4166666803226,-12.3256628518316));
#6882=CARTESIAN_POINT('Ctrl Pts',(-39.8371685740842,35.2083333469893,-23.));
#6883=CARTESIAN_POINT('Ctrl Pts',(-33.6743371481684,35.0000000136559,-33.6743371481684));
#6884=CARTESIAN_POINT('Ctrl Pts',(-23.,34.7916666803226,-39.8371685740842));
#6885=CARTESIAN_POINT('Ctrl Pts',(-12.3256628518317,34.5833333469893,-46.));
#6886=CARTESIAN_POINT('Ctrl Pts',(-2.81668763803891E-15,34.3750000136559,
-46.));
#6887=CARTESIAN_POINT('Ctrl Pts',(12.3256628518316,34.1666666803226,-46.));
#6888=CARTESIAN_POINT('Ctrl Pts',(23.,33.9583333469893,-39.8371685740842));
#6889=CARTESIAN_POINT('Ctrl Pts',(33.6743371481683,33.7500000136559,-33.6743371481684));
#6890=CARTESIAN_POINT('Ctrl Pts',(39.8371685740842,33.5416666803226,-23.));
#6891=CARTESIAN_POINT('Ctrl Pts',(46.,33.3333333469893,-12.3256628518317));
#6892=CARTESIAN_POINT('Ctrl Pts',(46.,33.1250000136559,-5.63337527607782E-15));
#6893=CARTESIAN_POINT('Ctrl Pts',(46.,32.9166666803226,12.3256628518316));
#6894=CARTESIAN_POINT('Ctrl Pts',(39.8371685740842,32.7083333469893,23.));
#6895=CARTESIAN_POINT('Ctrl Pts',(33.6743371481684,32.5000000136559,33.6743371481683));
#6896=CARTESIAN_POINT('Ctrl Pts',(23.,32.2916666803226,39.8371685740842));
#6897=CARTESIAN_POINT('Ctrl Pts',(12.3256628518317,32.0833333469893,46.));
#6898=CARTESIAN_POINT('Ctrl Pts',(8.45006291411674E-15,31.8750000136559,
46.));
#6899=CARTESIAN_POINT('Ctrl Pts',(-12.3256628518316,31.6666666803226,46.));
#6900=CARTESIAN_POINT('Ctrl Pts',(-23.,31.4583333469893,39.8371685740842));
#6901=CARTESIAN_POINT('Ctrl Pts',(-33.6743371481683,31.2500000136559,33.6743371481684));
#6902=CARTESIAN_POINT('Ctrl Pts',(-39.8371685740842,31.0416666803226,23.));
#6903=CARTESIAN_POINT('Ctrl Pts',(-46.,30.8333333469893,12.3256628518317));
#6904=CARTESIAN_POINT('Ctrl Pts',(-46.,30.6250000136559,0.));
#6905=CARTESIAN_POINT('Ctrl Pts',(-46.,30.4166666803226,-12.3256628518316));
#6906=CARTESIAN_POINT('Ctrl Pts',(-39.8371685740842,30.2083333469893,-23.));
#6907=CARTESIAN_POINT('Ctrl Pts',(-33.6743371481684,30.0000000136559,-33.6743371481684));
#6908=CARTESIAN_POINT('Ctrl Pts',(-23.,29.7916666803226,-39.8371685740842));
#6909=CARTESIAN_POINT('Ctrl Pts',(-12.3256628518317,29.5833333469893,-46.));
#6910=CARTESIAN_POINT('Ctrl Pts',(-2.81668763803891E-15,29.3750000136559,
-46.));
#6911=CARTESIAN_POINT('Ctrl Pts',(12.3256628518316,29.1666666803226,-46.));
#6912=CARTESIAN_POINT('Ctrl Pts',(23.,28.9583333469893,-39.8371685740842));
#6913=CARTESIAN_POINT('Ctrl Pts',(33.6743371481683,28.7500000136559,-33.6743371481684));
#6914=CARTESIAN_POINT('Ctrl Pts',(39.8371685740842,28.5416666803226,-23.));
#6915=CARTESIAN_POINT('Ctrl Pts',(46.,28.3333333469893,-12.3256628518317));
#6916=CARTESIAN_POINT('Ctrl Pts',(46.,28.1250000136559,-5.63337527607782E-15));
#6917=CARTESIAN_POINT('Ctrl Pts',(46.,27.9166666803226,12.3256628518316));
#6918=CARTESIAN_POINT('Ctrl Pts',(39.8371685740842,27.7083333469893,23.));
#6919=CARTESIAN_POINT('Ctrl Pts',(33.6743371481684,27.5000000136559,33.6743371481683));
#6920=CARTESIAN_POINT('Ctrl Pts',(23.,27.2916666803226,39.8371685740842));
#6921=CARTESIAN_POINT('Ctrl Pts',(12.3256628518317,27.0833333469893,46.));
#6922=CARTESIAN_POINT('Ctrl Pts',(8.45006291411674E-15,26.8750000136559,
46.));
#6923=CARTESIAN_POINT('Ctrl Pts',(-12.3256628518316,26.6666666803226,46.));
#6924=CARTESIAN_POINT('Ctrl Pts',(-23.,26.4583333469893,39.8371685740842));
#6925=CARTESIAN_POINT('Ctrl Pts',(-33.6743371481683,26.2500000136559,33.6743371481684));
#6926=CARTESIAN_POINT('Ctrl Pts',(-39.8371685740842,26.0416666803226,23.));
#6927=CARTESIAN_POINT('Ctrl Pts',(-46.,25.8333333469893,12.3256628518317));
#6928=CARTESIAN_POINT('Ctrl Pts',(-46.,25.6250000136559,0.));
#6929=CARTESIAN_POINT('Ctrl Pts',(-48.706329375,57.187500006828,-1.8898197019151E-14));
#6930=CARTESIAN_POINT('Ctrl Pts',(-48.706329375,56.9791666734946,-13.0508216223155));
#6931=CARTESIAN_POINT('Ctrl Pts',(-42.1809185638422,56.7708333401613,-24.3531646875));
#6932=CARTESIAN_POINT('Ctrl Pts',(-35.6555077526845,56.562500006828,-35.6555077526845));
#6933=CARTESIAN_POINT('Ctrl Pts',(-24.3531646875,56.3541666734946,-42.1809185638423));
#6934=CARTESIAN_POINT('Ctrl Pts',(-13.0508216223155,56.1458333401613,-48.706329375));
#6935=CARTESIAN_POINT('Ctrl Pts',(1.59157945007855E-14,55.937500006828,
-48.706329375));
#6936=CARTESIAN_POINT('Ctrl Pts',(13.0508216223155,55.7291666734946,-48.706329375));
#6937=CARTESIAN_POINT('Ctrl Pts',(24.3531646875,55.5208333401613,-42.1809185638422));
#6938=CARTESIAN_POINT('Ctrl Pts',(35.6555077526845,55.312500006828,-35.6555077526845));
#6939=CARTESIAN_POINT('Ctrl Pts',(42.1809185638422,55.1041666734946,-24.3531646875));
#6940=CARTESIAN_POINT('Ctrl Pts',(48.706329375,54.8958333401613,-13.0508216223155));
#6941=CARTESIAN_POINT('Ctrl Pts',(48.706329375,54.687500006828,1.293339198242E-14));
#6942=CARTESIAN_POINT('Ctrl Pts',(48.706329375,54.4791666734946,13.0508216223155));
#6943=CARTESIAN_POINT('Ctrl Pts',(42.1809185638422,54.2708333401613,24.3531646875));
#6944=CARTESIAN_POINT('Ctrl Pts',(35.6555077526845,54.062500006828,35.6555077526845));
#6945=CARTESIAN_POINT('Ctrl Pts',(24.3531646875,53.8541666734946,42.1809185638422));
#6946=CARTESIAN_POINT('Ctrl Pts',(13.0508216223155,53.6458333401613,48.706329375));
#6947=CARTESIAN_POINT('Ctrl Pts',(-9.95098946405443E-15,53.437500006828,
48.706329375));
#6948=CARTESIAN_POINT('Ctrl Pts',(-13.0508216223155,53.2291666734946,48.706329375));
#6949=CARTESIAN_POINT('Ctrl Pts',(-24.3531646875,53.0208333401613,42.1809185638423));
#6950=CARTESIAN_POINT('Ctrl Pts',(-35.6555077526845,52.812500006828,35.6555077526845));
#6951=CARTESIAN_POINT('Ctrl Pts',(-42.1809185638422,52.6041666734946,24.3531646875));
#6952=CARTESIAN_POINT('Ctrl Pts',(-48.706329375,52.3958333401613,13.0508216223155));
#6953=CARTESIAN_POINT('Ctrl Pts',(-48.706329375,52.187500006828,-1.8898197019151E-14));
#6954=CARTESIAN_POINT('Ctrl Pts',(-48.706329375,51.9791666734946,-13.0508216223155));
#6955=CARTESIAN_POINT('Ctrl Pts',(-42.1809185638422,51.7708333401613,-24.3531646875));
#6956=CARTESIAN_POINT('Ctrl Pts',(-35.6555077526845,51.562500006828,-35.6555077526845));
#6957=CARTESIAN_POINT('Ctrl Pts',(-24.3531646875,51.3541666734946,-42.1809185638423));
#6958=CARTESIAN_POINT('Ctrl Pts',(-13.0508216223155,51.1458333401613,-48.706329375));
#6959=CARTESIAN_POINT('Ctrl Pts',(1.59157945007855E-14,50.937500006828,
-48.706329375));
#6960=CARTESIAN_POINT('Ctrl Pts',(13.0508216223155,50.7291666734946,-48.706329375));
#6961=CARTESIAN_POINT('Ctrl Pts',(24.3531646875,50.5208333401613,-42.1809185638422));
#6962=CARTESIAN_POINT('Ctrl Pts',(35.6555077526845,50.312500006828,-35.6555077526845));
#6963=CARTESIAN_POINT('Ctrl Pts',(42.1809185638422,50.1041666734946,-24.3531646875));
#6964=CARTESIAN_POINT('Ctrl Pts',(48.706329375,49.8958333401613,-13.0508216223155));
#6965=CARTESIAN_POINT('Ctrl Pts',(48.706329375,49.687500006828,1.293339198242E-14));
#6966=CARTESIAN_POINT('Ctrl Pts',(48.706329375,49.4791666734946,13.0508216223155));
#6967=CARTESIAN_POINT('Ctrl Pts',(42.1809185638422,49.2708333401613,24.3531646875));
#6968=CARTESIAN_POINT('Ctrl Pts',(35.6555077526845,49.062500006828,35.6555077526845));
#6969=CARTESIAN_POINT('Ctrl Pts',(24.3531646875,48.8541666734946,42.1809185638422));
#6970=CARTESIAN_POINT('Ctrl Pts',(13.0508216223155,48.6458333401613,48.706329375));
#6971=CARTESIAN_POINT('Ctrl Pts',(-9.95098946405443E-15,48.437500006828,
48.706329375));
#6972=CARTESIAN_POINT('Ctrl Pts',(-13.0508216223155,48.2291666734946,48.706329375));
#6973=CARTESIAN_POINT('Ctrl Pts',(-24.3531646875,48.0208333401613,42.1809185638423));
#6974=CARTESIAN_POINT('Ctrl Pts',(-35.6555077526845,47.812500006828,35.6555077526845));
#6975=CARTESIAN_POINT('Ctrl Pts',(-42.1809185638422,47.6041666734946,24.3531646875));
#6976=CARTESIAN_POINT('Ctrl Pts',(-48.706329375,47.3958333401613,13.0508216223155));
#6977=CARTESIAN_POINT('Ctrl Pts',(-48.706329375,47.187500006828,-1.8898197019151E-14));
#6978=CARTESIAN_POINT('Ctrl Pts',(-48.706329375,46.9791666734946,-13.0508216223155));
#6979=CARTESIAN_POINT('Ctrl Pts',(-42.1809185638422,46.7708333401613,-24.3531646875));
#6980=CARTESIAN_POINT('Ctrl Pts',(-35.6555077526845,46.562500006828,-35.6555077526845));
#6981=CARTESIAN_POINT('Ctrl Pts',(-24.3531646875,46.3541666734946,-42.1809185638423));
#6982=CARTESIAN_POINT('Ctrl Pts',(-13.0508216223155,46.1458333401613,-48.706329375));
#6983=CARTESIAN_POINT('Ctrl Pts',(1.59157945007855E-14,45.937500006828,
-48.706329375));
#6984=CARTESIAN_POINT('Ctrl Pts',(13.0508216223155,45.7291666734946,-48.706329375));
#6985=CARTESIAN_POINT('Ctrl Pts',(24.3531646875,45.5208333401613,-42.1809185638422));
#6986=CARTESIAN_POINT('Ctrl Pts',(35.6555077526845,45.312500006828,-35.6555077526845));
#6987=CARTESIAN_POINT('Ctrl Pts',(42.1809185638422,45.1041666734946,-24.3531646875));
#6988=CARTESIAN_POINT('Ctrl Pts',(48.706329375,44.8958333401613,-13.0508216223155));
#6989=CARTESIAN_POINT('Ctrl Pts',(48.706329375,44.687500006828,1.293339198242E-14));
#6990=CARTESIAN_POINT('Ctrl Pts',(48.706329375,44.4791666734946,13.0508216223155));
#6991=CARTESIAN_POINT('Ctrl Pts',(42.1809185638422,44.2708333401613,24.3531646875));
#6992=CARTESIAN_POINT('Ctrl Pts',(35.6555077526845,44.062500006828,35.6555077526845));
#6993=CARTESIAN_POINT('Ctrl Pts',(24.3531646875,43.8541666734946,42.1809185638422));
#6994=CARTESIAN_POINT('Ctrl Pts',(13.0508216223155,43.6458333401613,48.706329375));
#6995=CARTESIAN_POINT('Ctrl Pts',(-9.95098946405443E-15,43.437500006828,
48.706329375));
#6996=CARTESIAN_POINT('Ctrl Pts',(-13.0508216223155,43.2291666734946,48.706329375));
#6997=CARTESIAN_POINT('Ctrl Pts',(-24.3531646875,43.0208333401613,42.1809185638423));
#6998=CARTESIAN_POINT('Ctrl Pts',(-35.6555077526845,42.812500006828,35.6555077526845));
#6999=CARTESIAN_POINT('Ctrl Pts',(-42.1809185638422,42.6041666734946,24.3531646875));
#7000=CARTESIAN_POINT('Ctrl Pts',(-48.706329375,42.3958333401613,13.0508216223155));
#7001=CARTESIAN_POINT('Ctrl Pts',(-48.706329375,42.187500006828,-1.8898197019151E-14));
#7002=CARTESIAN_POINT('Ctrl Pts',(-48.706329375,41.9791666734946,-13.0508216223155));
#7003=CARTESIAN_POINT('Ctrl Pts',(-42.1809185638422,41.7708333401613,-24.3531646875));
#7004=CARTESIAN_POINT('Ctrl Pts',(-35.6555077526845,41.562500006828,-35.6555077526845));
#7005=CARTESIAN_POINT('Ctrl Pts',(-24.3531646875,41.3541666734946,-42.1809185638423));
#7006=CARTESIAN_POINT('Ctrl Pts',(-13.0508216223155,41.1458333401613,-48.706329375));
#7007=CARTESIAN_POINT('Ctrl Pts',(1.59157945007855E-14,40.937500006828,
-48.706329375));
#7008=CARTESIAN_POINT('Ctrl Pts',(13.0508216223155,40.7291666734946,-48.706329375));
#7009=CARTESIAN_POINT('Ctrl Pts',(24.3531646875,40.5208333401613,-42.1809185638422));
#7010=CARTESIAN_POINT('Ctrl Pts',(35.6555077526845,40.312500006828,-35.6555077526845));
#7011=CARTESIAN_POINT('Ctrl Pts',(42.1809185638422,40.1041666734946,-24.3531646875));
#7012=CARTESIAN_POINT('Ctrl Pts',(48.706329375,39.8958333401613,-13.0508216223155));
#7013=CARTESIAN_POINT('Ctrl Pts',(48.706329375,39.687500006828,1.293339198242E-14));
#7014=CARTESIAN_POINT('Ctrl Pts',(48.706329375,39.4791666734946,13.0508216223155));
#7015=CARTESIAN_POINT('Ctrl Pts',(42.1809185638422,39.2708333401613,24.3531646875));
#7016=CARTESIAN_POINT('Ctrl Pts',(35.6555077526845,39.062500006828,35.6555077526845));
#7017=CARTESIAN_POINT('Ctrl Pts',(24.3531646875,38.8541666734946,42.1809185638422));
#7018=CARTESIAN_POINT('Ctrl Pts',(13.0508216223155,38.6458333401613,48.706329375));
#7019=CARTESIAN_POINT('Ctrl Pts',(-9.95098946405443E-15,38.437500006828,
48.706329375));
#7020=CARTESIAN_POINT('Ctrl Pts',(-13.0508216223155,38.2291666734946,48.706329375));
#7021=CARTESIAN_POINT('Ctrl Pts',(-24.3531646875,38.0208333401613,42.1809185638423));
#7022=CARTESIAN_POINT('Ctrl Pts',(-35.6555077526845,37.812500006828,35.6555077526845));
#7023=CARTESIAN_POINT('Ctrl Pts',(-42.1809185638422,37.6041666734946,24.3531646875));
#7024=CARTESIAN_POINT('Ctrl Pts',(-48.706329375,37.3958333401613,13.0508216223155));
#7025=CARTESIAN_POINT('Ctrl Pts',(-48.706329375,37.187500006828,-1.8898197019151E-14));
#7026=CARTESIAN_POINT('Ctrl Pts',(-48.706329375,36.9791666734946,-13.0508216223155));
#7027=CARTESIAN_POINT('Ctrl Pts',(-42.1809185638422,36.7708333401613,-24.3531646875));
#7028=CARTESIAN_POINT('Ctrl Pts',(-35.6555077526845,36.562500006828,-35.6555077526845));
#7029=CARTESIAN_POINT('Ctrl Pts',(-24.3531646875,36.3541666734946,-42.1809185638423));
#7030=CARTESIAN_POINT('Ctrl Pts',(-13.0508216223155,36.1458333401613,-48.706329375));
#7031=CARTESIAN_POINT('Ctrl Pts',(1.59157945007855E-14,35.937500006828,
-48.706329375));
#7032=CARTESIAN_POINT('Ctrl Pts',(13.0508216223155,35.7291666734946,-48.706329375));
#7033=CARTESIAN_POINT('Ctrl Pts',(24.3531646875,35.5208333401613,-42.1809185638422));
#7034=CARTESIAN_POINT('Ctrl Pts',(35.6555077526845,35.312500006828,-35.6555077526845));
#7035=CARTESIAN_POINT('Ctrl Pts',(42.1809185638422,35.1041666734946,-24.3531646875));
#7036=CARTESIAN_POINT('Ctrl Pts',(48.706329375,34.8958333401613,-13.0508216223155));
#7037=CARTESIAN_POINT('Ctrl Pts',(48.706329375,34.687500006828,1.293339198242E-14));
#7038=CARTESIAN_POINT('Ctrl Pts',(48.706329375,34.4791666734946,13.0508216223155));
#7039=CARTESIAN_POINT('Ctrl Pts',(42.1809185638422,34.2708333401613,24.3531646875));
#7040=CARTESIAN_POINT('Ctrl Pts',(35.6555077526845,34.062500006828,35.6555077526845));
#7041=CARTESIAN_POINT('Ctrl Pts',(24.3531646875,33.8541666734946,42.1809185638422));
#7042=CARTESIAN_POINT('Ctrl Pts',(13.0508216223155,33.6458333401613,48.706329375));
#7043=CARTESIAN_POINT('Ctrl Pts',(-9.95098946405443E-15,33.437500006828,
48.706329375));
#7044=CARTESIAN_POINT('Ctrl Pts',(-13.0508216223155,33.2291666734946,48.706329375));
#7045=CARTESIAN_POINT('Ctrl Pts',(-24.3531646875,33.0208333401613,42.1809185638423));
#7046=CARTESIAN_POINT('Ctrl Pts',(-35.6555077526845,32.812500006828,35.6555077526845));
#7047=CARTESIAN_POINT('Ctrl Pts',(-42.1809185638422,32.6041666734946,24.3531646875));
#7048=CARTESIAN_POINT('Ctrl Pts',(-48.706329375,32.3958333401613,13.0508216223155));
#7049=CARTESIAN_POINT('Ctrl Pts',(-48.706329375,32.187500006828,-1.8898197019151E-14));
#7050=CARTESIAN_POINT('Ctrl Pts',(-48.706329375,31.9791666734946,-13.0508216223155));
#7051=CARTESIAN_POINT('Ctrl Pts',(-42.1809185638422,31.7708333401613,-24.3531646875));
#7052=CARTESIAN_POINT('Ctrl Pts',(-35.6555077526845,31.562500006828,-35.6555077526845));
#7053=CARTESIAN_POINT('Ctrl Pts',(-24.3531646875,31.3541666734946,-42.1809185638423));
#7054=CARTESIAN_POINT('Ctrl Pts',(-13.0508216223155,31.1458333401613,-48.706329375));
#7055=CARTESIAN_POINT('Ctrl Pts',(1.59157945007855E-14,30.937500006828,
-48.706329375));
#7056=CARTESIAN_POINT('Ctrl Pts',(13.0508216223155,30.7291666734946,-48.706329375));
#7057=CARTESIAN_POINT('Ctrl Pts',(24.3531646875,30.5208333401613,-42.1809185638422));
#7058=CARTESIAN_POINT('Ctrl Pts',(35.6555077526845,30.312500006828,-35.6555077526845));
#7059=CARTESIAN_POINT('Ctrl Pts',(42.1809185638422,30.1041666734946,-24.3531646875));
#7060=CARTESIAN_POINT('Ctrl Pts',(48.706329375,29.8958333401613,-13.0508216223155));
#7061=CARTESIAN_POINT('Ctrl Pts',(48.706329375,29.687500006828,1.293339198242E-14));
#7062=CARTESIAN_POINT('Ctrl Pts',(48.706329375,29.4791666734946,13.0508216223155));
#7063=CARTESIAN_POINT('Ctrl Pts',(42.1809185638422,29.2708333401613,24.3531646875));
#7064=CARTESIAN_POINT('Ctrl Pts',(35.6555077526845,29.062500006828,35.6555077526845));
#7065=CARTESIAN_POINT('Ctrl Pts',(24.3531646875,28.8541666734946,42.1809185638422));
#7066=CARTESIAN_POINT('Ctrl Pts',(13.0508216223155,28.6458333401613,48.706329375));
#7067=CARTESIAN_POINT('Ctrl Pts',(-9.95098946405443E-15,28.437500006828,
48.706329375));
#7068=CARTESIAN_POINT('Ctrl Pts',(-13.0508216223155,28.2291666734946,48.706329375));
#7069=CARTESIAN_POINT('Ctrl Pts',(-24.3531646875,28.0208333401613,42.1809185638423));
#7070=CARTESIAN_POINT('Ctrl Pts',(-35.6555077526845,27.812500006828,35.6555077526845));
#7071=CARTESIAN_POINT('Ctrl Pts',(-42.1809185638422,27.6041666734946,24.3531646875));
#7072=CARTESIAN_POINT('Ctrl Pts',(-48.706329375,27.3958333401613,13.0508216223155));
#7073=CARTESIAN_POINT('Ctrl Pts',(-48.706329375,27.187500006828,-1.8898197019151E-14));
#7074=CARTESIAN_POINT('',(3.61292728433799,45.8792520480092,-48.5721450795008));
#7075=CARTESIAN_POINT('',(48.5134353784345,44.7574536451604,-4.33048599679671));
#7076=CARTESIAN_POINT('Ctrl Pts',(3.61292728433799,45.8792520480092,-48.5721450795008));
#7077=CARTESIAN_POINT('Ctrl Pts',(14.7133549689477,45.6985216017706,-47.7464652997852));
#7078=CARTESIAN_POINT('Ctrl Pts',(24.3531646875,45.5208333401613,-42.1809185638422));
#7079=CARTESIAN_POINT('Ctrl Pts',(35.6555077526845,45.312500006828,-35.6555077526845));
#7080=CARTESIAN_POINT('Ctrl Pts',(42.1809185638422,45.1041666734946,-24.3531646875));
#7081=CARTESIAN_POINT('Ctrl Pts',(47.5573898704235,44.9325149229327,-15.0408432190651));
#7082=CARTESIAN_POINT('Ctrl Pts',(48.5134353784345,44.7574536451604,-4.33048599679671));
#7083=CARTESIAN_POINT('Origin',(-4513.8089981458,7998.28355101971,-4.33048637721644));
#7084=CARTESIAN_POINT('Ctrl Pts',(3.61292728433799,44.3132892765089,-45.8578974271399));
#7085=CARTESIAN_POINT('Ctrl Pts',(3.61292728433796,44.4468822859549,-46.089460636719));
#7086=CARTESIAN_POINT('Ctrl Pts',(3.61292728433805,44.7140705280012,-46.5525857733052));
#7087=CARTESIAN_POINT('Ctrl Pts',(3.61292728433797,44.9812630238616,-47.0157084557285));
#7088=CARTESIAN_POINT('Ctrl Pts',(3.61292728433797,45.3696539378594,-47.6888965792834));
#7089=CARTESIAN_POINT('Ctrl Pts',(3.61292728433799,45.624451287085,-48.1305218136162));
#7090=CARTESIAN_POINT('Ctrl Pts',(3.61292728433799,45.8792520480092,-48.5721450795008));
#7091=CARTESIAN_POINT('Ctrl Pts',(-46.,55.6250000136559,0.));
#7092=CARTESIAN_POINT('Ctrl Pts',(-46.,55.4166666803226,-12.3256628518316));
#7093=CARTESIAN_POINT('Ctrl Pts',(-39.8371685740842,55.2083333469893,-23.));
#7094=CARTESIAN_POINT('Ctrl Pts',(-33.6743371481684,55.0000000136559,-33.6743371481684));
#7095=CARTESIAN_POINT('Ctrl Pts',(-23.,54.7916666803226,-39.8371685740842));
#7096=CARTESIAN_POINT('Ctrl Pts',(-12.3256628518317,54.5833333469893,-46.));
#7097=CARTESIAN_POINT('Ctrl Pts',(-2.81668763803891E-15,54.3750000136559,
-46.));
#7098=CARTESIAN_POINT('Ctrl Pts',(12.3256628518316,54.1666666803226,-46.));
#7099=CARTESIAN_POINT('Ctrl Pts',(23.,53.9583333469893,-39.8371685740842));
#7100=CARTESIAN_POINT('Ctrl Pts',(33.6743371481683,53.7500000136559,-33.6743371481684));
#7101=CARTESIAN_POINT('Ctrl Pts',(39.8371685740842,53.5416666803226,-23.));
#7102=CARTESIAN_POINT('Ctrl Pts',(46.,53.3333333469893,-12.3256628518317));
#7103=CARTESIAN_POINT('Ctrl Pts',(46.,53.1250000136559,-5.63337527607782E-15));
#7104=CARTESIAN_POINT('Ctrl Pts',(46.,52.9166666803226,12.3256628518316));
#7105=CARTESIAN_POINT('Ctrl Pts',(39.8371685740842,52.7083333469893,23.));
#7106=CARTESIAN_POINT('Ctrl Pts',(33.6743371481684,52.5000000136559,33.6743371481683));
#7107=CARTESIAN_POINT('Ctrl Pts',(23.,52.2916666803226,39.8371685740842));
#7108=CARTESIAN_POINT('Ctrl Pts',(12.3256628518317,52.0833333469893,46.));
#7109=CARTESIAN_POINT('Ctrl Pts',(8.45006291411674E-15,51.8750000136559,
46.));
#7110=CARTESIAN_POINT('Ctrl Pts',(-12.3256628518316,51.6666666803226,46.));
#7111=CARTESIAN_POINT('Ctrl Pts',(-23.,51.4583333469893,39.8371685740842));
#7112=CARTESIAN_POINT('Ctrl Pts',(-33.6743371481683,51.2500000136559,33.6743371481684));
#7113=CARTESIAN_POINT('Ctrl Pts',(-39.8371685740842,51.0416666803226,23.));
#7114=CARTESIAN_POINT('Ctrl Pts',(-46.,50.8333333469893,12.3256628518317));
#7115=CARTESIAN_POINT('Ctrl Pts',(-46.,50.6250000136559,0.));
#7116=CARTESIAN_POINT('Ctrl Pts',(-46.,50.4166666803226,-12.3256628518316));
#7117=CARTESIAN_POINT('Ctrl Pts',(-39.8371685740842,50.2083333469893,-23.));
#7118=CARTESIAN_POINT('Ctrl Pts',(-33.6743371481684,50.0000000136559,-33.6743371481684));
#7119=CARTESIAN_POINT('Ctrl Pts',(-23.,49.7916666803226,-39.8371685740842));
#7120=CARTESIAN_POINT('Ctrl Pts',(-12.3256628518317,49.5833333469893,-46.));
#7121=CARTESIAN_POINT('Ctrl Pts',(-2.81668763803891E-15,49.3750000136559,
-46.));
#7122=CARTESIAN_POINT('Ctrl Pts',(12.3256628518316,49.1666666803226,-46.));
#7123=CARTESIAN_POINT('Ctrl Pts',(23.,48.9583333469893,-39.8371685740842));
#7124=CARTESIAN_POINT('Ctrl Pts',(33.6743371481683,48.7500000136559,-33.6743371481684));
#7125=CARTESIAN_POINT('Ctrl Pts',(39.8371685740842,48.5416666803226,-23.));
#7126=CARTESIAN_POINT('Ctrl Pts',(46.,48.3333333469893,-12.3256628518317));
#7127=CARTESIAN_POINT('Ctrl Pts',(46.,48.1250000136559,-5.63337527607782E-15));
#7128=CARTESIAN_POINT('Ctrl Pts',(46.,47.9166666803226,12.3256628518316));
#7129=CARTESIAN_POINT('Ctrl Pts',(39.8371685740842,47.7083333469893,23.));
#7130=CARTESIAN_POINT('Ctrl Pts',(33.6743371481684,47.5000000136559,33.6743371481683));
#7131=CARTESIAN_POINT('Ctrl Pts',(23.,47.2916666803226,39.8371685740842));
#7132=CARTESIAN_POINT('Ctrl Pts',(12.3256628518317,47.0833333469893,46.));
#7133=CARTESIAN_POINT('Ctrl Pts',(8.45006291411674E-15,46.8750000136559,
46.));
#7134=CARTESIAN_POINT('Ctrl Pts',(-12.3256628518316,46.6666666803226,46.));
#7135=CARTESIAN_POINT('Ctrl Pts',(-23.,46.4583333469893,39.8371685740842));
#7136=CARTESIAN_POINT('Ctrl Pts',(-33.6743371481683,46.2500000136559,33.6743371481684));
#7137=CARTESIAN_POINT('Ctrl Pts',(-39.8371685740842,46.0416666803226,23.));
#7138=CARTESIAN_POINT('Ctrl Pts',(-46.,45.8333333469892,12.3256628518317));
#7139=CARTESIAN_POINT('Ctrl Pts',(-46.,45.6250000136559,0.));
#7140=CARTESIAN_POINT('Ctrl Pts',(-46.,45.4166666803226,-12.3256628518316));
#7141=CARTESIAN_POINT('Ctrl Pts',(-39.8371685740842,45.2083333469893,-23.));
#7142=CARTESIAN_POINT('Ctrl Pts',(-33.6743371481684,45.0000000136559,-33.6743371481684));
#7143=CARTESIAN_POINT('Ctrl Pts',(-23.,44.7916666803226,-39.8371685740842));
#7144=CARTESIAN_POINT('Ctrl Pts',(-12.3256628518317,44.5833333469893,-46.));
#7145=CARTESIAN_POINT('Ctrl Pts',(-2.81668763803891E-15,44.3750000136559,
-46.));
#7146=CARTESIAN_POINT('Ctrl Pts',(12.3256628518316,44.1666666803226,-46.));
#7147=CARTESIAN_POINT('Ctrl Pts',(23.,43.9583333469893,-39.8371685740842));
#7148=CARTESIAN_POINT('Ctrl Pts',(33.6743371481683,43.7500000136559,-33.6743371481684));
#7149=CARTESIAN_POINT('Ctrl Pts',(39.8371685740842,43.5416666803226,-23.));
#7150=CARTESIAN_POINT('Ctrl Pts',(46.,43.3333333469893,-12.3256628518317));
#7151=CARTESIAN_POINT('Ctrl Pts',(46.,43.1250000136559,-5.63337527607782E-15));
#7152=CARTESIAN_POINT('Ctrl Pts',(46.,42.9166666803226,12.3256628518316));
#7153=CARTESIAN_POINT('Ctrl Pts',(39.8371685740842,42.7083333469893,23.));
#7154=CARTESIAN_POINT('Ctrl Pts',(33.6743371481684,42.5000000136559,33.6743371481683));
#7155=CARTESIAN_POINT('Ctrl Pts',(23.,42.2916666803226,39.8371685740842));
#7156=CARTESIAN_POINT('Ctrl Pts',(12.3256628518317,42.0833333469893,46.));
#7157=CARTESIAN_POINT('Ctrl Pts',(8.45006291411674E-15,41.8750000136559,
46.));
#7158=CARTESIAN_POINT('Ctrl Pts',(-12.3256628518316,41.6666666803226,46.));
#7159=CARTESIAN_POINT('Ctrl Pts',(-23.,41.4583333469893,39.8371685740842));
#7160=CARTESIAN_POINT('Ctrl Pts',(-33.6743371481683,41.2500000136559,33.6743371481684));
#7161=CARTESIAN_POINT('Ctrl Pts',(-39.8371685740842,41.0416666803226,23.));
#7162=CARTESIAN_POINT('Ctrl Pts',(-46.,40.8333333469893,12.3256628518317));
#7163=CARTESIAN_POINT('Ctrl Pts',(-46.,40.6250000136559,0.));
#7164=CARTESIAN_POINT('Ctrl Pts',(-46.,40.4166666803226,-12.3256628518316));
#7165=CARTESIAN_POINT('Ctrl Pts',(-39.8371685740842,40.2083333469893,-23.));
#7166=CARTESIAN_POINT('Ctrl Pts',(-33.6743371481684,40.0000000136559,-33.6743371481684));
#7167=CARTESIAN_POINT('Ctrl Pts',(-23.,39.7916666803226,-39.8371685740842));
#7168=CARTESIAN_POINT('Ctrl Pts',(-12.3256628518317,39.5833333469893,-46.));
#7169=CARTESIAN_POINT('Ctrl Pts',(-2.81668763803891E-15,39.3750000136559,
-46.));
#7170=CARTESIAN_POINT('Ctrl Pts',(12.3256628518316,39.1666666803226,-46.));
#7171=CARTESIAN_POINT('Ctrl Pts',(23.,38.9583333469893,-39.8371685740842));
#7172=CARTESIAN_POINT('Ctrl Pts',(33.6743371481683,38.7500000136559,-33.6743371481684));
#7173=CARTESIAN_POINT('Ctrl Pts',(39.8371685740842,38.5416666803226,-23.));
#7174=CARTESIAN_POINT('Ctrl Pts',(46.,38.3333333469893,-12.3256628518317));
#7175=CARTESIAN_POINT('Ctrl Pts',(46.,38.1250000136559,-5.63337527607782E-15));
#7176=CARTESIAN_POINT('Ctrl Pts',(46.,37.9166666803226,12.3256628518316));
#7177=CARTESIAN_POINT('Ctrl Pts',(39.8371685740842,37.7083333469893,23.));
#7178=CARTESIAN_POINT('Ctrl Pts',(33.6743371481684,37.5000000136559,33.6743371481683));
#7179=CARTESIAN_POINT('Ctrl Pts',(23.,37.2916666803226,39.8371685740842));
#7180=CARTESIAN_POINT('Ctrl Pts',(12.3256628518317,37.0833333469893,46.));
#7181=CARTESIAN_POINT('Ctrl Pts',(8.45006291411674E-15,36.8750000136559,
46.));
#7182=CARTESIAN_POINT('Ctrl Pts',(-12.3256628518316,36.6666666803226,46.));
#7183=CARTESIAN_POINT('Ctrl Pts',(-23.,36.4583333469893,39.8371685740842));
#7184=CARTESIAN_POINT('Ctrl Pts',(-33.6743371481683,36.2500000136559,33.6743371481684));
#7185=CARTESIAN_POINT('Ctrl Pts',(-39.8371685740842,36.0416666803226,23.));
#7186=CARTESIAN_POINT('Ctrl Pts',(-46.,35.8333333469893,12.3256628518317));
#7187=CARTESIAN_POINT('Ctrl Pts',(-46.,35.6250000136559,0.));
#7188=CARTESIAN_POINT('Ctrl Pts',(-46.,35.4166666803226,-12.3256628518316));
#7189=CARTESIAN_POINT('Ctrl Pts',(-39.8371685740842,35.2083333469893,-23.));
#7190=CARTESIAN_POINT('Ctrl Pts',(-33.6743371481684,35.0000000136559,-33.6743371481684));
#7191=CARTESIAN_POINT('Ctrl Pts',(-23.,34.7916666803226,-39.8371685740842));
#7192=CARTESIAN_POINT('Ctrl Pts',(-12.3256628518317,34.5833333469893,-46.));
#7193=CARTESIAN_POINT('Ctrl Pts',(-2.81668763803891E-15,34.3750000136559,
-46.));
#7194=CARTESIAN_POINT('Ctrl Pts',(12.3256628518316,34.1666666803226,-46.));
#7195=CARTESIAN_POINT('Ctrl Pts',(23.,33.9583333469893,-39.8371685740842));
#7196=CARTESIAN_POINT('Ctrl Pts',(33.6743371481683,33.7500000136559,-33.6743371481684));
#7197=CARTESIAN_POINT('Ctrl Pts',(39.8371685740842,33.5416666803226,-23.));
#7198=CARTESIAN_POINT('Ctrl Pts',(46.,33.3333333469893,-12.3256628518317));
#7199=CARTESIAN_POINT('Ctrl Pts',(46.,33.1250000136559,-5.63337527607782E-15));
#7200=CARTESIAN_POINT('Ctrl Pts',(46.,32.9166666803226,12.3256628518316));
#7201=CARTESIAN_POINT('Ctrl Pts',(39.8371685740842,32.7083333469893,23.));
#7202=CARTESIAN_POINT('Ctrl Pts',(33.6743371481684,32.5000000136559,33.6743371481683));
#7203=CARTESIAN_POINT('Ctrl Pts',(23.,32.2916666803226,39.8371685740842));
#7204=CARTESIAN_POINT('Ctrl Pts',(12.3256628518317,32.0833333469893,46.));
#7205=CARTESIAN_POINT('Ctrl Pts',(8.45006291411674E-15,31.8750000136559,
46.));
#7206=CARTESIAN_POINT('Ctrl Pts',(-12.3256628518316,31.6666666803226,46.));
#7207=CARTESIAN_POINT('Ctrl Pts',(-23.,31.4583333469893,39.8371685740842));
#7208=CARTESIAN_POINT('Ctrl Pts',(-33.6743371481683,31.2500000136559,33.6743371481684));
#7209=CARTESIAN_POINT('Ctrl Pts',(-39.8371685740842,31.0416666803226,23.));
#7210=CARTESIAN_POINT('Ctrl Pts',(-46.,30.8333333469893,12.3256628518317));
#7211=CARTESIAN_POINT('Ctrl Pts',(-46.,30.6250000136559,0.));
#7212=CARTESIAN_POINT('Ctrl Pts',(-46.,30.4166666803226,-12.3256628518316));
#7213=CARTESIAN_POINT('Ctrl Pts',(-39.8371685740842,30.2083333469893,-23.));
#7214=CARTESIAN_POINT('Ctrl Pts',(-33.6743371481684,30.0000000136559,-33.6743371481684));
#7215=CARTESIAN_POINT('Ctrl Pts',(-23.,29.7916666803226,-39.8371685740842));
#7216=CARTESIAN_POINT('Ctrl Pts',(-12.3256628518317,29.5833333469893,-46.));
#7217=CARTESIAN_POINT('Ctrl Pts',(-2.81668763803891E-15,29.3750000136559,
-46.));
#7218=CARTESIAN_POINT('Ctrl Pts',(12.3256628518316,29.1666666803226,-46.));
#7219=CARTESIAN_POINT('Ctrl Pts',(23.,28.9583333469893,-39.8371685740842));
#7220=CARTESIAN_POINT('Ctrl Pts',(33.6743371481683,28.7500000136559,-33.6743371481684));
#7221=CARTESIAN_POINT('Ctrl Pts',(39.8371685740842,28.5416666803226,-23.));
#7222=CARTESIAN_POINT('Ctrl Pts',(46.,28.3333333469893,-12.3256628518317));
#7223=CARTESIAN_POINT('Ctrl Pts',(46.,28.1250000136559,-5.63337527607782E-15));
#7224=CARTESIAN_POINT('Ctrl Pts',(46.,27.9166666803226,12.3256628518316));
#7225=CARTESIAN_POINT('Ctrl Pts',(39.8371685740842,27.7083333469893,23.));
#7226=CARTESIAN_POINT('Ctrl Pts',(33.6743371481684,27.5000000136559,33.6743371481683));
#7227=CARTESIAN_POINT('Ctrl Pts',(23.,27.2916666803226,39.8371685740842));
#7228=CARTESIAN_POINT('Ctrl Pts',(12.3256628518317,27.0833333469893,46.));
#7229=CARTESIAN_POINT('Ctrl Pts',(8.45006291411674E-15,26.8750000136559,
46.));
#7230=CARTESIAN_POINT('Ctrl Pts',(-12.3256628518316,26.6666666803226,46.));
#7231=CARTESIAN_POINT('Ctrl Pts',(-23.,26.4583333469893,39.8371685740842));
#7232=CARTESIAN_POINT('Ctrl Pts',(-33.6743371481683,26.2500000136559,33.6743371481684));
#7233=CARTESIAN_POINT('Ctrl Pts',(-39.8371685740842,26.0416666803226,23.));
#7234=CARTESIAN_POINT('Ctrl Pts',(-46.,25.8333333469893,12.3256628518317));
#7235=CARTESIAN_POINT('Ctrl Pts',(-46.,25.6250000136559,0.));
#7236=CARTESIAN_POINT('Ctrl Pts',(-48.706329375,57.187500006828,-1.8898197019151E-14));
#7237=CARTESIAN_POINT('Ctrl Pts',(-48.706329375,56.9791666734946,-13.0508216223155));
#7238=CARTESIAN_POINT('Ctrl Pts',(-42.1809185638422,56.7708333401613,-24.3531646875));
#7239=CARTESIAN_POINT('Ctrl Pts',(-35.6555077526845,56.562500006828,-35.6555077526845));
#7240=CARTESIAN_POINT('Ctrl Pts',(-24.3531646875,56.3541666734946,-42.1809185638423));
#7241=CARTESIAN_POINT('Ctrl Pts',(-13.0508216223155,56.1458333401613,-48.706329375));
#7242=CARTESIAN_POINT('Ctrl Pts',(1.59157945007855E-14,55.937500006828,
-48.706329375));
#7243=CARTESIAN_POINT('Ctrl Pts',(13.0508216223155,55.7291666734946,-48.706329375));
#7244=CARTESIAN_POINT('Ctrl Pts',(24.3531646875,55.5208333401613,-42.1809185638422));
#7245=CARTESIAN_POINT('Ctrl Pts',(35.6555077526845,55.312500006828,-35.6555077526845));
#7246=CARTESIAN_POINT('Ctrl Pts',(42.1809185638422,55.1041666734946,-24.3531646875));
#7247=CARTESIAN_POINT('Ctrl Pts',(48.706329375,54.8958333401613,-13.0508216223155));
#7248=CARTESIAN_POINT('Ctrl Pts',(48.706329375,54.687500006828,1.293339198242E-14));
#7249=CARTESIAN_POINT('Ctrl Pts',(48.706329375,54.4791666734946,13.0508216223155));
#7250=CARTESIAN_POINT('Ctrl Pts',(42.1809185638422,54.2708333401613,24.3531646875));
#7251=CARTESIAN_POINT('Ctrl Pts',(35.6555077526845,54.062500006828,35.6555077526845));
#7252=CARTESIAN_POINT('Ctrl Pts',(24.3531646875,53.8541666734946,42.1809185638422));
#7253=CARTESIAN_POINT('Ctrl Pts',(13.0508216223155,53.6458333401613,48.706329375));
#7254=CARTESIAN_POINT('Ctrl Pts',(-9.95098946405443E-15,53.437500006828,
48.706329375));
#7255=CARTESIAN_POINT('Ctrl Pts',(-13.0508216223155,53.2291666734946,48.706329375));
#7256=CARTESIAN_POINT('Ctrl Pts',(-24.3531646875,53.0208333401613,42.1809185638423));
#7257=CARTESIAN_POINT('Ctrl Pts',(-35.6555077526845,52.812500006828,35.6555077526845));
#7258=CARTESIAN_POINT('Ctrl Pts',(-42.1809185638422,52.6041666734946,24.3531646875));
#7259=CARTESIAN_POINT('Ctrl Pts',(-48.706329375,52.3958333401613,13.0508216223155));
#7260=CARTESIAN_POINT('Ctrl Pts',(-48.706329375,52.187500006828,-1.8898197019151E-14));
#7261=CARTESIAN_POINT('Ctrl Pts',(-48.706329375,51.9791666734946,-13.0508216223155));
#7262=CARTESIAN_POINT('Ctrl Pts',(-42.1809185638422,51.7708333401613,-24.3531646875));
#7263=CARTESIAN_POINT('Ctrl Pts',(-35.6555077526845,51.562500006828,-35.6555077526845));
#7264=CARTESIAN_POINT('Ctrl Pts',(-24.3531646875,51.3541666734946,-42.1809185638423));
#7265=CARTESIAN_POINT('Ctrl Pts',(-13.0508216223155,51.1458333401613,-48.706329375));
#7266=CARTESIAN_POINT('Ctrl Pts',(1.59157945007855E-14,50.937500006828,
-48.706329375));
#7267=CARTESIAN_POINT('Ctrl Pts',(13.0508216223155,50.7291666734946,-48.706329375));
#7268=CARTESIAN_POINT('Ctrl Pts',(24.3531646875,50.5208333401613,-42.1809185638422));
#7269=CARTESIAN_POINT('Ctrl Pts',(35.6555077526845,50.312500006828,-35.6555077526845));
#7270=CARTESIAN_POINT('Ctrl Pts',(42.1809185638422,50.1041666734946,-24.3531646875));
#7271=CARTESIAN_POINT('Ctrl Pts',(48.706329375,49.8958333401613,-13.0508216223155));
#7272=CARTESIAN_POINT('Ctrl Pts',(48.706329375,49.687500006828,1.293339198242E-14));
#7273=CARTESIAN_POINT('Ctrl Pts',(48.706329375,49.4791666734946,13.0508216223155));
#7274=CARTESIAN_POINT('Ctrl Pts',(42.1809185638422,49.2708333401613,24.3531646875));
#7275=CARTESIAN_POINT('Ctrl Pts',(35.6555077526845,49.062500006828,35.6555077526845));
#7276=CARTESIAN_POINT('Ctrl Pts',(24.3531646875,48.8541666734946,42.1809185638422));
#7277=CARTESIAN_POINT('Ctrl Pts',(13.0508216223155,48.6458333401613,48.706329375));
#7278=CARTESIAN_POINT('Ctrl Pts',(-9.95098946405443E-15,48.437500006828,
48.706329375));
#7279=CARTESIAN_POINT('Ctrl Pts',(-13.0508216223155,48.2291666734946,48.706329375));
#7280=CARTESIAN_POINT('Ctrl Pts',(-24.3531646875,48.0208333401613,42.1809185638423));
#7281=CARTESIAN_POINT('Ctrl Pts',(-35.6555077526845,47.812500006828,35.6555077526845));
#7282=CARTESIAN_POINT('Ctrl Pts',(-42.1809185638422,47.6041666734946,24.3531646875));
#7283=CARTESIAN_POINT('Ctrl Pts',(-48.706329375,47.3958333401613,13.0508216223155));
#7284=CARTESIAN_POINT('Ctrl Pts',(-48.706329375,47.187500006828,-1.8898197019151E-14));
#7285=CARTESIAN_POINT('Ctrl Pts',(-48.706329375,46.9791666734946,-13.0508216223155));
#7286=CARTESIAN_POINT('Ctrl Pts',(-42.1809185638422,46.7708333401613,-24.3531646875));
#7287=CARTESIAN_POINT('Ctrl Pts',(-35.6555077526845,46.562500006828,-35.6555077526845));
#7288=CARTESIAN_POINT('Ctrl Pts',(-24.3531646875,46.3541666734946,-42.1809185638423));
#7289=CARTESIAN_POINT('Ctrl Pts',(-13.0508216223155,46.1458333401613,-48.706329375));
#7290=CARTESIAN_POINT('Ctrl Pts',(1.59157945007855E-14,45.937500006828,
-48.706329375));
#7291=CARTESIAN_POINT('Ctrl Pts',(13.0508216223155,45.7291666734946,-48.706329375));
#7292=CARTESIAN_POINT('Ctrl Pts',(24.3531646875,45.5208333401613,-42.1809185638422));
#7293=CARTESIAN_POINT('Ctrl Pts',(35.6555077526845,45.312500006828,-35.6555077526845));
#7294=CARTESIAN_POINT('Ctrl Pts',(42.1809185638422,45.1041666734946,-24.3531646875));
#7295=CARTESIAN_POINT('Ctrl Pts',(48.706329375,44.8958333401613,-13.0508216223155));
#7296=CARTESIAN_POINT('Ctrl Pts',(48.706329375,44.687500006828,1.293339198242E-14));
#7297=CARTESIAN_POINT('Ctrl Pts',(48.706329375,44.4791666734946,13.0508216223155));
#7298=CARTESIAN_POINT('Ctrl Pts',(42.1809185638422,44.2708333401613,24.3531646875));
#7299=CARTESIAN_POINT('Ctrl Pts',(35.6555077526845,44.062500006828,35.6555077526845));
#7300=CARTESIAN_POINT('Ctrl Pts',(24.3531646875,43.8541666734946,42.1809185638422));
#7301=CARTESIAN_POINT('Ctrl Pts',(13.0508216223155,43.6458333401613,48.706329375));
#7302=CARTESIAN_POINT('Ctrl Pts',(-9.95098946405443E-15,43.437500006828,
48.706329375));
#7303=CARTESIAN_POINT('Ctrl Pts',(-13.0508216223155,43.2291666734946,48.706329375));
#7304=CARTESIAN_POINT('Ctrl Pts',(-24.3531646875,43.0208333401613,42.1809185638423));
#7305=CARTESIAN_POINT('Ctrl Pts',(-35.6555077526845,42.812500006828,35.6555077526845));
#7306=CARTESIAN_POINT('Ctrl Pts',(-42.1809185638422,42.6041666734946,24.3531646875));
#7307=CARTESIAN_POINT('Ctrl Pts',(-48.706329375,42.3958333401613,13.0508216223155));
#7308=CARTESIAN_POINT('Ctrl Pts',(-48.706329375,42.187500006828,-1.8898197019151E-14));
#7309=CARTESIAN_POINT('Ctrl Pts',(-48.706329375,41.9791666734946,-13.0508216223155));
#7310=CARTESIAN_POINT('Ctrl Pts',(-42.1809185638422,41.7708333401613,-24.3531646875));
#7311=CARTESIAN_POINT('Ctrl Pts',(-35.6555077526845,41.562500006828,-35.6555077526845));
#7312=CARTESIAN_POINT('Ctrl Pts',(-24.3531646875,41.3541666734946,-42.1809185638423));
#7313=CARTESIAN_POINT('Ctrl Pts',(-13.0508216223155,41.1458333401613,-48.706329375));
#7314=CARTESIAN_POINT('Ctrl Pts',(1.59157945007855E-14,40.937500006828,
-48.706329375));
#7315=CARTESIAN_POINT('Ctrl Pts',(13.0508216223155,40.7291666734946,-48.706329375));
#7316=CARTESIAN_POINT('Ctrl Pts',(24.3531646875,40.5208333401613,-42.1809185638422));
#7317=CARTESIAN_POINT('Ctrl Pts',(35.6555077526845,40.312500006828,-35.6555077526845));
#7318=CARTESIAN_POINT('Ctrl Pts',(42.1809185638422,40.1041666734946,-24.3531646875));
#7319=CARTESIAN_POINT('Ctrl Pts',(48.706329375,39.8958333401613,-13.0508216223155));
#7320=CARTESIAN_POINT('Ctrl Pts',(48.706329375,39.687500006828,1.293339198242E-14));
#7321=CARTESIAN_POINT('Ctrl Pts',(48.706329375,39.4791666734946,13.0508216223155));
#7322=CARTESIAN_POINT('Ctrl Pts',(42.1809185638422,39.2708333401613,24.3531646875));
#7323=CARTESIAN_POINT('Ctrl Pts',(35.6555077526845,39.062500006828,35.6555077526845));
#7324=CARTESIAN_POINT('Ctrl Pts',(24.3531646875,38.8541666734946,42.1809185638422));
#7325=CARTESIAN_POINT('Ctrl Pts',(13.0508216223155,38.6458333401613,48.706329375));
#7326=CARTESIAN_POINT('Ctrl Pts',(-9.95098946405443E-15,38.437500006828,
48.706329375));
#7327=CARTESIAN_POINT('Ctrl Pts',(-13.0508216223155,38.2291666734946,48.706329375));
#7328=CARTESIAN_POINT('Ctrl Pts',(-24.3531646875,38.0208333401613,42.1809185638423));
#7329=CARTESIAN_POINT('Ctrl Pts',(-35.6555077526845,37.812500006828,35.6555077526845));
#7330=CARTESIAN_POINT('Ctrl Pts',(-42.1809185638422,37.6041666734946,24.3531646875));
#7331=CARTESIAN_POINT('Ctrl Pts',(-48.706329375,37.3958333401613,13.0508216223155));
#7332=CARTESIAN_POINT('Ctrl Pts',(-48.706329375,37.187500006828,-1.8898197019151E-14));
#7333=CARTESIAN_POINT('Ctrl Pts',(-48.706329375,36.9791666734946,-13.0508216223155));
#7334=CARTESIAN_POINT('Ctrl Pts',(-42.1809185638422,36.7708333401613,-24.3531646875));
#7335=CARTESIAN_POINT('Ctrl Pts',(-35.6555077526845,36.562500006828,-35.6555077526845));
#7336=CARTESIAN_POINT('Ctrl Pts',(-24.3531646875,36.3541666734946,-42.1809185638423));
#7337=CARTESIAN_POINT('Ctrl Pts',(-13.0508216223155,36.1458333401613,-48.706329375));
#7338=CARTESIAN_POINT('Ctrl Pts',(1.59157945007855E-14,35.937500006828,
-48.706329375));
#7339=CARTESIAN_POINT('Ctrl Pts',(13.0508216223155,35.7291666734946,-48.706329375));
#7340=CARTESIAN_POINT('Ctrl Pts',(24.3531646875,35.5208333401613,-42.1809185638422));
#7341=CARTESIAN_POINT('Ctrl Pts',(35.6555077526845,35.312500006828,-35.6555077526845));
#7342=CARTESIAN_POINT('Ctrl Pts',(42.1809185638422,35.1041666734946,-24.3531646875));
#7343=CARTESIAN_POINT('Ctrl Pts',(48.706329375,34.8958333401613,-13.0508216223155));
#7344=CARTESIAN_POINT('Ctrl Pts',(48.706329375,34.687500006828,1.293339198242E-14));
#7345=CARTESIAN_POINT('Ctrl Pts',(48.706329375,34.4791666734946,13.0508216223155));
#7346=CARTESIAN_POINT('Ctrl Pts',(42.1809185638422,34.2708333401613,24.3531646875));
#7347=CARTESIAN_POINT('Ctrl Pts',(35.6555077526845,34.062500006828,35.6555077526845));
#7348=CARTESIAN_POINT('Ctrl Pts',(24.3531646875,33.8541666734946,42.1809185638422));
#7349=CARTESIAN_POINT('Ctrl Pts',(13.0508216223155,33.6458333401613,48.706329375));
#7350=CARTESIAN_POINT('Ctrl Pts',(-9.95098946405443E-15,33.437500006828,
48.706329375));
#7351=CARTESIAN_POINT('Ctrl Pts',(-13.0508216223155,33.2291666734946,48.706329375));
#7352=CARTESIAN_POINT('Ctrl Pts',(-24.3531646875,33.0208333401613,42.1809185638423));
#7353=CARTESIAN_POINT('Ctrl Pts',(-35.6555077526845,32.812500006828,35.6555077526845));
#7354=CARTESIAN_POINT('Ctrl Pts',(-42.1809185638422,32.6041666734946,24.3531646875));
#7355=CARTESIAN_POINT('Ctrl Pts',(-48.706329375,32.3958333401613,13.0508216223155));
#7356=CARTESIAN_POINT('Ctrl Pts',(-48.706329375,32.187500006828,-1.8898197019151E-14));
#7357=CARTESIAN_POINT('Ctrl Pts',(-48.706329375,31.9791666734946,-13.0508216223155));
#7358=CARTESIAN_POINT('Ctrl Pts',(-42.1809185638422,31.7708333401613,-24.3531646875));
#7359=CARTESIAN_POINT('Ctrl Pts',(-35.6555077526845,31.562500006828,-35.6555077526845));
#7360=CARTESIAN_POINT('Ctrl Pts',(-24.3531646875,31.3541666734946,-42.1809185638423));
#7361=CARTESIAN_POINT('Ctrl Pts',(-13.0508216223155,31.1458333401613,-48.706329375));
#7362=CARTESIAN_POINT('Ctrl Pts',(1.59157945007855E-14,30.937500006828,
-48.706329375));
#7363=CARTESIAN_POINT('Ctrl Pts',(13.0508216223155,30.7291666734946,-48.706329375));
#7364=CARTESIAN_POINT('Ctrl Pts',(24.3531646875,30.5208333401613,-42.1809185638422));
#7365=CARTESIAN_POINT('Ctrl Pts',(35.6555077526845,30.312500006828,-35.6555077526845));
#7366=CARTESIAN_POINT('Ctrl Pts',(42.1809185638422,30.1041666734946,-24.3531646875));
#7367=CARTESIAN_POINT('Ctrl Pts',(48.706329375,29.8958333401613,-13.0508216223155));
#7368=CARTESIAN_POINT('Ctrl Pts',(48.706329375,29.687500006828,1.293339198242E-14));
#7369=CARTESIAN_POINT('Ctrl Pts',(48.706329375,29.4791666734946,13.0508216223155));
#7370=CARTESIAN_POINT('Ctrl Pts',(42.1809185638422,29.2708333401613,24.3531646875));
#7371=CARTESIAN_POINT('Ctrl Pts',(35.6555077526845,29.062500006828,35.6555077526845));
#7372=CARTESIAN_POINT('Ctrl Pts',(24.3531646875,28.8541666734946,42.1809185638422));
#7373=CARTESIAN_POINT('Ctrl Pts',(13.0508216223155,28.6458333401613,48.706329375));
#7374=CARTESIAN_POINT('Ctrl Pts',(-9.95098946405443E-15,28.437500006828,
48.706329375));
#7375=CARTESIAN_POINT('Ctrl Pts',(-13.0508216223155,28.2291666734946,48.706329375));
#7376=CARTESIAN_POINT('Ctrl Pts',(-24.3531646875,28.0208333401613,42.1809185638423));
#7377=CARTESIAN_POINT('Ctrl Pts',(-35.6555077526845,27.812500006828,35.6555077526845));
#7378=CARTESIAN_POINT('Ctrl Pts',(-42.1809185638422,27.6041666734946,24.3531646875));
#7379=CARTESIAN_POINT('Ctrl Pts',(-48.706329375,27.3958333401613,13.0508216223155));
#7380=CARTESIAN_POINT('Ctrl Pts',(-48.706329375,27.187500006828,-1.8898197019151E-14));
#7381=CARTESIAN_POINT('',(48.5725845633798,44.6293483229262,3.60701400320328));
#7382=CARTESIAN_POINT('Ctrl Pts',(45.858362923034,43.0633913333999,3.60701400320327));
#7383=CARTESIAN_POINT('Ctrl Pts',(46.089925771934,43.1969849680263,3.60701400320324));
#7384=CARTESIAN_POINT('Ctrl Pts',(46.5530501979845,43.4641744416604,3.60701400320326));
#7385=CARTESIAN_POINT('Ctrl Pts',(47.0161721905706,43.7313681332063,3.60701400320324));
#7386=CARTESIAN_POINT('Ctrl Pts',(47.6893519862319,44.1197565257476,3.60701400320324));
#7387=CARTESIAN_POINT('Ctrl Pts',(48.1309692507095,44.3745507329179,3.60701400320328));
#7388=CARTESIAN_POINT('Ctrl Pts',(48.5725845633798,44.6293483229262,3.60701400320328));
#7389=CARTESIAN_POINT('',(3.61292728433797,43.4957479656467,48.5721450795008));
#7390=CARTESIAN_POINT('Ctrl Pts',(48.5725845633798,44.6293483229262,3.60701400320328));
#7391=CARTESIAN_POINT('Ctrl Pts',(47.7480251419552,44.4485714020251,14.7106532430575));
#7392=CARTESIAN_POINT('Ctrl Pts',(42.1809185638422,44.2708333401613,24.3531646875));
#7393=CARTESIAN_POINT('Ctrl Pts',(35.6555077526845,44.062500006828,35.6555077526845));
#7394=CARTESIAN_POINT('Ctrl Pts',(24.3531646875,43.8541666734946,42.1809185638422));
#7395=CARTESIAN_POINT('Ctrl Pts',(14.7133549689477,43.6764784118853,47.7464652997852));
#7396=CARTESIAN_POINT('Ctrl Pts',(3.61292728433797,43.4957479656467,48.5721450795008));
#7397=CARTESIAN_POINT('Ctrl Pts',(3.61292728433797,43.4957479656467,48.5721450795008));
#7398=CARTESIAN_POINT('Ctrl Pts',(3.61292728433797,43.3625660950884,48.3403451622818));
#7399=CARTESIAN_POINT('Ctrl Pts',(3.612927284338,43.2293911846469,48.1085412459393));
#7400=CARTESIAN_POINT('Ctrl Pts',(3.612927284338,42.9630558994543,47.6449250631479));
#7401=CARTESIAN_POINT('Ctrl Pts',(3.61292728433804,42.8298955244832,47.4131127965212));
#7402=CARTESIAN_POINT('Ctrl Pts',(3.61292728433804,42.6967427432646,47.1812961682826));
#7403=CARTESIAN_POINT('Ctrl Pts',(3.61292728433804,42.4433704509922,46.7401795055579));
#7404=CARTESIAN_POINT('Ctrl Pts',(3.61292728433798,42.1900256371662,46.2990470581854));
#7405=CARTESIAN_POINT('Ctrl Pts',(3.61292728433799,41.936710750803,45.8578974271399));
#7406=CARTESIAN_POINT('Ctrl Pts',(-46.,55.6250000136559,0.));
#7407=CARTESIAN_POINT('Ctrl Pts',(-46.,55.4166666803226,-12.3256628518316));
#7408=CARTESIAN_POINT('Ctrl Pts',(-39.8371685740842,55.2083333469893,-23.));
#7409=CARTESIAN_POINT('Ctrl Pts',(-33.6743371481684,55.0000000136559,-33.6743371481684));
#7410=CARTESIAN_POINT('Ctrl Pts',(-23.,54.7916666803226,-39.8371685740842));
#7411=CARTESIAN_POINT('Ctrl Pts',(-12.3256628518317,54.5833333469893,-46.));
#7412=CARTESIAN_POINT('Ctrl Pts',(-2.81668763803891E-15,54.3750000136559,
-46.));
#7413=CARTESIAN_POINT('Ctrl Pts',(12.3256628518316,54.1666666803226,-46.));
#7414=CARTESIAN_POINT('Ctrl Pts',(23.,53.9583333469893,-39.8371685740842));
#7415=CARTESIAN_POINT('Ctrl Pts',(33.6743371481683,53.7500000136559,-33.6743371481684));
#7416=CARTESIAN_POINT('Ctrl Pts',(39.8371685740842,53.5416666803226,-23.));
#7417=CARTESIAN_POINT('Ctrl Pts',(46.,53.3333333469893,-12.3256628518317));
#7418=CARTESIAN_POINT('Ctrl Pts',(46.,53.1250000136559,-5.63337527607782E-15));
#7419=CARTESIAN_POINT('Ctrl Pts',(46.,52.9166666803226,12.3256628518316));
#7420=CARTESIAN_POINT('Ctrl Pts',(39.8371685740842,52.7083333469893,23.));
#7421=CARTESIAN_POINT('Ctrl Pts',(33.6743371481684,52.5000000136559,33.6743371481683));
#7422=CARTESIAN_POINT('Ctrl Pts',(23.,52.2916666803226,39.8371685740842));
#7423=CARTESIAN_POINT('Ctrl Pts',(12.3256628518317,52.0833333469893,46.));
#7424=CARTESIAN_POINT('Ctrl Pts',(8.45006291411674E-15,51.8750000136559,
46.));
#7425=CARTESIAN_POINT('Ctrl Pts',(-12.3256628518316,51.6666666803226,46.));
#7426=CARTESIAN_POINT('Ctrl Pts',(-23.,51.4583333469893,39.8371685740842));
#7427=CARTESIAN_POINT('Ctrl Pts',(-33.6743371481683,51.2500000136559,33.6743371481684));
#7428=CARTESIAN_POINT('Ctrl Pts',(-39.8371685740842,51.0416666803226,23.));
#7429=CARTESIAN_POINT('Ctrl Pts',(-46.,50.8333333469893,12.3256628518317));
#7430=CARTESIAN_POINT('Ctrl Pts',(-46.,50.6250000136559,0.));
#7431=CARTESIAN_POINT('Ctrl Pts',(-46.,50.4166666803226,-12.3256628518316));
#7432=CARTESIAN_POINT('Ctrl Pts',(-39.8371685740842,50.2083333469893,-23.));
#7433=CARTESIAN_POINT('Ctrl Pts',(-33.6743371481684,50.0000000136559,-33.6743371481684));
#7434=CARTESIAN_POINT('Ctrl Pts',(-23.,49.7916666803226,-39.8371685740842));
#7435=CARTESIAN_POINT('Ctrl Pts',(-12.3256628518317,49.5833333469893,-46.));
#7436=CARTESIAN_POINT('Ctrl Pts',(-2.81668763803891E-15,49.3750000136559,
-46.));
#7437=CARTESIAN_POINT('Ctrl Pts',(12.3256628518316,49.1666666803226,-46.));
#7438=CARTESIAN_POINT('Ctrl Pts',(23.,48.9583333469893,-39.8371685740842));
#7439=CARTESIAN_POINT('Ctrl Pts',(33.6743371481683,48.7500000136559,-33.6743371481684));
#7440=CARTESIAN_POINT('Ctrl Pts',(39.8371685740842,48.5416666803226,-23.));
#7441=CARTESIAN_POINT('Ctrl Pts',(46.,48.3333333469893,-12.3256628518317));
#7442=CARTESIAN_POINT('Ctrl Pts',(46.,48.1250000136559,-5.63337527607782E-15));
#7443=CARTESIAN_POINT('Ctrl Pts',(46.,47.9166666803226,12.3256628518316));
#7444=CARTESIAN_POINT('Ctrl Pts',(39.8371685740842,47.7083333469893,23.));
#7445=CARTESIAN_POINT('Ctrl Pts',(33.6743371481684,47.5000000136559,33.6743371481683));
#7446=CARTESIAN_POINT('Ctrl Pts',(23.,47.2916666803226,39.8371685740842));
#7447=CARTESIAN_POINT('Ctrl Pts',(12.3256628518317,47.0833333469893,46.));
#7448=CARTESIAN_POINT('Ctrl Pts',(8.45006291411674E-15,46.8750000136559,
46.));
#7449=CARTESIAN_POINT('Ctrl Pts',(-12.3256628518316,46.6666666803226,46.));
#7450=CARTESIAN_POINT('Ctrl Pts',(-23.,46.4583333469893,39.8371685740842));
#7451=CARTESIAN_POINT('Ctrl Pts',(-33.6743371481683,46.2500000136559,33.6743371481684));
#7452=CARTESIAN_POINT('Ctrl Pts',(-39.8371685740842,46.0416666803226,23.));
#7453=CARTESIAN_POINT('Ctrl Pts',(-46.,45.8333333469892,12.3256628518317));
#7454=CARTESIAN_POINT('Ctrl Pts',(-46.,45.6250000136559,0.));
#7455=CARTESIAN_POINT('Ctrl Pts',(-46.,45.4166666803226,-12.3256628518316));
#7456=CARTESIAN_POINT('Ctrl Pts',(-39.8371685740842,45.2083333469893,-23.));
#7457=CARTESIAN_POINT('Ctrl Pts',(-33.6743371481684,45.0000000136559,-33.6743371481684));
#7458=CARTESIAN_POINT('Ctrl Pts',(-23.,44.7916666803226,-39.8371685740842));
#7459=CARTESIAN_POINT('Ctrl Pts',(-12.3256628518317,44.5833333469893,-46.));
#7460=CARTESIAN_POINT('Ctrl Pts',(-2.81668763803891E-15,44.3750000136559,
-46.));
#7461=CARTESIAN_POINT('Ctrl Pts',(12.3256628518316,44.1666666803226,-46.));
#7462=CARTESIAN_POINT('Ctrl Pts',(23.,43.9583333469893,-39.8371685740842));
#7463=CARTESIAN_POINT('Ctrl Pts',(33.6743371481683,43.7500000136559,-33.6743371481684));
#7464=CARTESIAN_POINT('Ctrl Pts',(39.8371685740842,43.5416666803226,-23.));
#7465=CARTESIAN_POINT('Ctrl Pts',(46.,43.3333333469893,-12.3256628518317));
#7466=CARTESIAN_POINT('Ctrl Pts',(46.,43.1250000136559,-5.63337527607782E-15));
#7467=CARTESIAN_POINT('Ctrl Pts',(46.,42.9166666803226,12.3256628518316));
#7468=CARTESIAN_POINT('Ctrl Pts',(39.8371685740842,42.7083333469893,23.));
#7469=CARTESIAN_POINT('Ctrl Pts',(33.6743371481684,42.5000000136559,33.6743371481683));
#7470=CARTESIAN_POINT('Ctrl Pts',(23.,42.2916666803226,39.8371685740842));
#7471=CARTESIAN_POINT('Ctrl Pts',(12.3256628518317,42.0833333469893,46.));
#7472=CARTESIAN_POINT('Ctrl Pts',(8.45006291411674E-15,41.8750000136559,
46.));
#7473=CARTESIAN_POINT('Ctrl Pts',(-12.3256628518316,41.6666666803226,46.));
#7474=CARTESIAN_POINT('Ctrl Pts',(-23.,41.4583333469893,39.8371685740842));
#7475=CARTESIAN_POINT('Ctrl Pts',(-33.6743371481683,41.2500000136559,33.6743371481684));
#7476=CARTESIAN_POINT('Ctrl Pts',(-39.8371685740842,41.0416666803226,23.));
#7477=CARTESIAN_POINT('Ctrl Pts',(-46.,40.8333333469893,12.3256628518317));
#7478=CARTESIAN_POINT('Ctrl Pts',(-46.,40.6250000136559,0.));
#7479=CARTESIAN_POINT('Ctrl Pts',(-46.,40.4166666803226,-12.3256628518316));
#7480=CARTESIAN_POINT('Ctrl Pts',(-39.8371685740842,40.2083333469893,-23.));
#7481=CARTESIAN_POINT('Ctrl Pts',(-33.6743371481684,40.0000000136559,-33.6743371481684));
#7482=CARTESIAN_POINT('Ctrl Pts',(-23.,39.7916666803226,-39.8371685740842));
#7483=CARTESIAN_POINT('Ctrl Pts',(-12.3256628518317,39.5833333469893,-46.));
#7484=CARTESIAN_POINT('Ctrl Pts',(-2.81668763803891E-15,39.3750000136559,
-46.));
#7485=CARTESIAN_POINT('Ctrl Pts',(12.3256628518316,39.1666666803226,-46.));
#7486=CARTESIAN_POINT('Ctrl Pts',(23.,38.9583333469893,-39.8371685740842));
#7487=CARTESIAN_POINT('Ctrl Pts',(33.6743371481683,38.7500000136559,-33.6743371481684));
#7488=CARTESIAN_POINT('Ctrl Pts',(39.8371685740842,38.5416666803226,-23.));
#7489=CARTESIAN_POINT('Ctrl Pts',(46.,38.3333333469893,-12.3256628518317));
#7490=CARTESIAN_POINT('Ctrl Pts',(46.,38.1250000136559,-5.63337527607782E-15));
#7491=CARTESIAN_POINT('Ctrl Pts',(46.,37.9166666803226,12.3256628518316));
#7492=CARTESIAN_POINT('Ctrl Pts',(39.8371685740842,37.7083333469893,23.));
#7493=CARTESIAN_POINT('Ctrl Pts',(33.6743371481684,37.5000000136559,33.6743371481683));
#7494=CARTESIAN_POINT('Ctrl Pts',(23.,37.2916666803226,39.8371685740842));
#7495=CARTESIAN_POINT('Ctrl Pts',(12.3256628518317,37.0833333469893,46.));
#7496=CARTESIAN_POINT('Ctrl Pts',(8.45006291411674E-15,36.8750000136559,
46.));
#7497=CARTESIAN_POINT('Ctrl Pts',(-12.3256628518316,36.6666666803226,46.));
#7498=CARTESIAN_POINT('Ctrl Pts',(-23.,36.4583333469893,39.8371685740842));
#7499=CARTESIAN_POINT('Ctrl Pts',(-33.6743371481683,36.2500000136559,33.6743371481684));
#7500=CARTESIAN_POINT('Ctrl Pts',(-39.8371685740842,36.0416666803226,23.));
#7501=CARTESIAN_POINT('Ctrl Pts',(-46.,35.8333333469893,12.3256628518317));
#7502=CARTESIAN_POINT('Ctrl Pts',(-46.,35.6250000136559,0.));
#7503=CARTESIAN_POINT('Ctrl Pts',(-46.,35.4166666803226,-12.3256628518316));
#7504=CARTESIAN_POINT('Ctrl Pts',(-39.8371685740842,35.2083333469893,-23.));
#7505=CARTESIAN_POINT('Ctrl Pts',(-33.6743371481684,35.0000000136559,-33.6743371481684));
#7506=CARTESIAN_POINT('Ctrl Pts',(-23.,34.7916666803226,-39.8371685740842));
#7507=CARTESIAN_POINT('Ctrl Pts',(-12.3256628518317,34.5833333469893,-46.));
#7508=CARTESIAN_POINT('Ctrl Pts',(-2.81668763803891E-15,34.3750000136559,
-46.));
#7509=CARTESIAN_POINT('Ctrl Pts',(12.3256628518316,34.1666666803226,-46.));
#7510=CARTESIAN_POINT('Ctrl Pts',(23.,33.9583333469893,-39.8371685740842));
#7511=CARTESIAN_POINT('Ctrl Pts',(33.6743371481683,33.7500000136559,-33.6743371481684));
#7512=CARTESIAN_POINT('Ctrl Pts',(39.8371685740842,33.5416666803226,-23.));
#7513=CARTESIAN_POINT('Ctrl Pts',(46.,33.3333333469893,-12.3256628518317));
#7514=CARTESIAN_POINT('Ctrl Pts',(46.,33.1250000136559,-5.63337527607782E-15));
#7515=CARTESIAN_POINT('Ctrl Pts',(46.,32.9166666803226,12.3256628518316));
#7516=CARTESIAN_POINT('Ctrl Pts',(39.8371685740842,32.7083333469893,23.));
#7517=CARTESIAN_POINT('Ctrl Pts',(33.6743371481684,32.5000000136559,33.6743371481683));
#7518=CARTESIAN_POINT('Ctrl Pts',(23.,32.2916666803226,39.8371685740842));
#7519=CARTESIAN_POINT('Ctrl Pts',(12.3256628518317,32.0833333469893,46.));
#7520=CARTESIAN_POINT('Ctrl Pts',(8.45006291411674E-15,31.8750000136559,
46.));
#7521=CARTESIAN_POINT('Ctrl Pts',(-12.3256628518316,31.6666666803226,46.));
#7522=CARTESIAN_POINT('Ctrl Pts',(-23.,31.4583333469893,39.8371685740842));
#7523=CARTESIAN_POINT('Ctrl Pts',(-33.6743371481683,31.2500000136559,33.6743371481684));
#7524=CARTESIAN_POINT('Ctrl Pts',(-39.8371685740842,31.0416666803226,23.));
#7525=CARTESIAN_POINT('Ctrl Pts',(-46.,30.8333333469893,12.3256628518317));
#7526=CARTESIAN_POINT('Ctrl Pts',(-46.,30.6250000136559,0.));
#7527=CARTESIAN_POINT('Ctrl Pts',(-46.,30.4166666803226,-12.3256628518316));
#7528=CARTESIAN_POINT('Ctrl Pts',(-39.8371685740842,30.2083333469893,-23.));
#7529=CARTESIAN_POINT('Ctrl Pts',(-33.6743371481684,30.0000000136559,-33.6743371481684));
#7530=CARTESIAN_POINT('Ctrl Pts',(-23.,29.7916666803226,-39.8371685740842));
#7531=CARTESIAN_POINT('Ctrl Pts',(-12.3256628518317,29.5833333469893,-46.));
#7532=CARTESIAN_POINT('Ctrl Pts',(-2.81668763803891E-15,29.3750000136559,
-46.));
#7533=CARTESIAN_POINT('Ctrl Pts',(12.3256628518316,29.1666666803226,-46.));
#7534=CARTESIAN_POINT('Ctrl Pts',(23.,28.9583333469893,-39.8371685740842));
#7535=CARTESIAN_POINT('Ctrl Pts',(33.6743371481683,28.7500000136559,-33.6743371481684));
#7536=CARTESIAN_POINT('Ctrl Pts',(39.8371685740842,28.5416666803226,-23.));
#7537=CARTESIAN_POINT('Ctrl Pts',(46.,28.3333333469893,-12.3256628518317));
#7538=CARTESIAN_POINT('Ctrl Pts',(46.,28.1250000136559,-5.63337527607782E-15));
#7539=CARTESIAN_POINT('Ctrl Pts',(46.,27.9166666803226,12.3256628518316));
#7540=CARTESIAN_POINT('Ctrl Pts',(39.8371685740842,27.7083333469893,23.));
#7541=CARTESIAN_POINT('Ctrl Pts',(33.6743371481684,27.5000000136559,33.6743371481683));
#7542=CARTESIAN_POINT('Ctrl Pts',(23.,27.2916666803226,39.8371685740842));
#7543=CARTESIAN_POINT('Ctrl Pts',(12.3256628518317,27.0833333469893,46.));
#7544=CARTESIAN_POINT('Ctrl Pts',(8.45006291411674E-15,26.8750000136559,
46.));
#7545=CARTESIAN_POINT('Ctrl Pts',(-12.3256628518316,26.6666666803226,46.));
#7546=CARTESIAN_POINT('Ctrl Pts',(-23.,26.4583333469893,39.8371685740842));
#7547=CARTESIAN_POINT('Ctrl Pts',(-33.6743371481683,26.2500000136559,33.6743371481684));
#7548=CARTESIAN_POINT('Ctrl Pts',(-39.8371685740842,26.0416666803226,23.));
#7549=CARTESIAN_POINT('Ctrl Pts',(-46.,25.8333333469893,12.3256628518317));
#7550=CARTESIAN_POINT('Ctrl Pts',(-46.,25.6250000136559,0.));
#7551=CARTESIAN_POINT('Ctrl Pts',(-48.706329375,57.187500006828,-1.8898197019151E-14));
#7552=CARTESIAN_POINT('Ctrl Pts',(-48.706329375,56.9791666734946,-13.0508216223155));
#7553=CARTESIAN_POINT('Ctrl Pts',(-42.1809185638422,56.7708333401613,-24.3531646875));
#7554=CARTESIAN_POINT('Ctrl Pts',(-35.6555077526845,56.562500006828,-35.6555077526845));
#7555=CARTESIAN_POINT('Ctrl Pts',(-24.3531646875,56.3541666734946,-42.1809185638423));
#7556=CARTESIAN_POINT('Ctrl Pts',(-13.0508216223155,56.1458333401613,-48.706329375));
#7557=CARTESIAN_POINT('Ctrl Pts',(1.59157945007855E-14,55.937500006828,
-48.706329375));
#7558=CARTESIAN_POINT('Ctrl Pts',(13.0508216223155,55.7291666734946,-48.706329375));
#7559=CARTESIAN_POINT('Ctrl Pts',(24.3531646875,55.5208333401613,-42.1809185638422));
#7560=CARTESIAN_POINT('Ctrl Pts',(35.6555077526845,55.312500006828,-35.6555077526845));
#7561=CARTESIAN_POINT('Ctrl Pts',(42.1809185638422,55.1041666734946,-24.3531646875));
#7562=CARTESIAN_POINT('Ctrl Pts',(48.706329375,54.8958333401613,-13.0508216223155));
#7563=CARTESIAN_POINT('Ctrl Pts',(48.706329375,54.687500006828,1.293339198242E-14));
#7564=CARTESIAN_POINT('Ctrl Pts',(48.706329375,54.4791666734946,13.0508216223155));
#7565=CARTESIAN_POINT('Ctrl Pts',(42.1809185638422,54.2708333401613,24.3531646875));
#7566=CARTESIAN_POINT('Ctrl Pts',(35.6555077526845,54.062500006828,35.6555077526845));
#7567=CARTESIAN_POINT('Ctrl Pts',(24.3531646875,53.8541666734946,42.1809185638422));
#7568=CARTESIAN_POINT('Ctrl Pts',(13.0508216223155,53.6458333401613,48.706329375));
#7569=CARTESIAN_POINT('Ctrl Pts',(-9.95098946405443E-15,53.437500006828,
48.706329375));
#7570=CARTESIAN_POINT('Ctrl Pts',(-13.0508216223155,53.2291666734946,48.706329375));
#7571=CARTESIAN_POINT('Ctrl Pts',(-24.3531646875,53.0208333401613,42.1809185638423));
#7572=CARTESIAN_POINT('Ctrl Pts',(-35.6555077526845,52.812500006828,35.6555077526845));
#7573=CARTESIAN_POINT('Ctrl Pts',(-42.1809185638422,52.6041666734946,24.3531646875));
#7574=CARTESIAN_POINT('Ctrl Pts',(-48.706329375,52.3958333401613,13.0508216223155));
#7575=CARTESIAN_POINT('Ctrl Pts',(-48.706329375,52.187500006828,-1.8898197019151E-14));
#7576=CARTESIAN_POINT('Ctrl Pts',(-48.706329375,51.9791666734946,-13.0508216223155));
#7577=CARTESIAN_POINT('Ctrl Pts',(-42.1809185638422,51.7708333401613,-24.3531646875));
#7578=CARTESIAN_POINT('Ctrl Pts',(-35.6555077526845,51.562500006828,-35.6555077526845));
#7579=CARTESIAN_POINT('Ctrl Pts',(-24.3531646875,51.3541666734946,-42.1809185638423));
#7580=CARTESIAN_POINT('Ctrl Pts',(-13.0508216223155,51.1458333401613,-48.706329375));
#7581=CARTESIAN_POINT('Ctrl Pts',(1.59157945007855E-14,50.937500006828,
-48.706329375));
#7582=CARTESIAN_POINT('Ctrl Pts',(13.0508216223155,50.7291666734946,-48.706329375));
#7583=CARTESIAN_POINT('Ctrl Pts',(24.3531646875,50.5208333401613,-42.1809185638422));
#7584=CARTESIAN_POINT('Ctrl Pts',(35.6555077526845,50.312500006828,-35.6555077526845));
#7585=CARTESIAN_POINT('Ctrl Pts',(42.1809185638422,50.1041666734946,-24.3531646875));
#7586=CARTESIAN_POINT('Ctrl Pts',(48.706329375,49.8958333401613,-13.0508216223155));
#7587=CARTESIAN_POINT('Ctrl Pts',(48.706329375,49.687500006828,1.293339198242E-14));
#7588=CARTESIAN_POINT('Ctrl Pts',(48.706329375,49.4791666734946,13.0508216223155));
#7589=CARTESIAN_POINT('Ctrl Pts',(42.1809185638422,49.2708333401613,24.3531646875));
#7590=CARTESIAN_POINT('Ctrl Pts',(35.6555077526845,49.062500006828,35.6555077526845));
#7591=CARTESIAN_POINT('Ctrl Pts',(24.3531646875,48.8541666734946,42.1809185638422));
#7592=CARTESIAN_POINT('Ctrl Pts',(13.0508216223155,48.6458333401613,48.706329375));
#7593=CARTESIAN_POINT('Ctrl Pts',(-9.95098946405443E-15,48.437500006828,
48.706329375));
#7594=CARTESIAN_POINT('Ctrl Pts',(-13.0508216223155,48.2291666734946,48.706329375));
#7595=CARTESIAN_POINT('Ctrl Pts',(-24.3531646875,48.0208333401613,42.1809185638423));
#7596=CARTESIAN_POINT('Ctrl Pts',(-35.6555077526845,47.812500006828,35.6555077526845));
#7597=CARTESIAN_POINT('Ctrl Pts',(-42.1809185638422,47.6041666734946,24.3531646875));
#7598=CARTESIAN_POINT('Ctrl Pts',(-48.706329375,47.3958333401613,13.0508216223155));
#7599=CARTESIAN_POINT('Ctrl Pts',(-48.706329375,47.187500006828,-1.8898197019151E-14));
#7600=CARTESIAN_POINT('Ctrl Pts',(-48.706329375,46.9791666734946,-13.0508216223155));
#7601=CARTESIAN_POINT('Ctrl Pts',(-42.1809185638422,46.7708333401613,-24.3531646875));
#7602=CARTESIAN_POINT('Ctrl Pts',(-35.6555077526845,46.562500006828,-35.6555077526845));
#7603=CARTESIAN_POINT('Ctrl Pts',(-24.3531646875,46.3541666734946,-42.1809185638423));
#7604=CARTESIAN_POINT('Ctrl Pts',(-13.0508216223155,46.1458333401613,-48.706329375));
#7605=CARTESIAN_POINT('Ctrl Pts',(1.59157945007855E-14,45.937500006828,
-48.706329375));
#7606=CARTESIAN_POINT('Ctrl Pts',(13.0508216223155,45.7291666734946,-48.706329375));
#7607=CARTESIAN_POINT('Ctrl Pts',(24.3531646875,45.5208333401613,-42.1809185638422));
#7608=CARTESIAN_POINT('Ctrl Pts',(35.6555077526845,45.312500006828,-35.6555077526845));
#7609=CARTESIAN_POINT('Ctrl Pts',(42.1809185638422,45.1041666734946,-24.3531646875));
#7610=CARTESIAN_POINT('Ctrl Pts',(48.706329375,44.8958333401613,-13.0508216223155));
#7611=CARTESIAN_POINT('Ctrl Pts',(48.706329375,44.687500006828,1.293339198242E-14));
#7612=CARTESIAN_POINT('Ctrl Pts',(48.706329375,44.4791666734946,13.0508216223155));
#7613=CARTESIAN_POINT('Ctrl Pts',(42.1809185638422,44.2708333401613,24.3531646875));
#7614=CARTESIAN_POINT('Ctrl Pts',(35.6555077526845,44.062500006828,35.6555077526845));
#7615=CARTESIAN_POINT('Ctrl Pts',(24.3531646875,43.8541666734946,42.1809185638422));
#7616=CARTESIAN_POINT('Ctrl Pts',(13.0508216223155,43.6458333401613,48.706329375));
#7617=CARTESIAN_POINT('Ctrl Pts',(-9.95098946405443E-15,43.437500006828,
48.706329375));
#7618=CARTESIAN_POINT('Ctrl Pts',(-13.0508216223155,43.2291666734946,48.706329375));
#7619=CARTESIAN_POINT('Ctrl Pts',(-24.3531646875,43.0208333401613,42.1809185638423));
#7620=CARTESIAN_POINT('Ctrl Pts',(-35.6555077526845,42.812500006828,35.6555077526845));
#7621=CARTESIAN_POINT('Ctrl Pts',(-42.1809185638422,42.6041666734946,24.3531646875));
#7622=CARTESIAN_POINT('Ctrl Pts',(-48.706329375,42.3958333401613,13.0508216223155));
#7623=CARTESIAN_POINT('Ctrl Pts',(-48.706329375,42.187500006828,-1.8898197019151E-14));
#7624=CARTESIAN_POINT('Ctrl Pts',(-48.706329375,41.9791666734946,-13.0508216223155));
#7625=CARTESIAN_POINT('Ctrl Pts',(-42.1809185638422,41.7708333401613,-24.3531646875));
#7626=CARTESIAN_POINT('Ctrl Pts',(-35.6555077526845,41.562500006828,-35.6555077526845));
#7627=CARTESIAN_POINT('Ctrl Pts',(-24.3531646875,41.3541666734946,-42.1809185638423));
#7628=CARTESIAN_POINT('Ctrl Pts',(-13.0508216223155,41.1458333401613,-48.706329375));
#7629=CARTESIAN_POINT('Ctrl Pts',(1.59157945007855E-14,40.937500006828,
-48.706329375));
#7630=CARTESIAN_POINT('Ctrl Pts',(13.0508216223155,40.7291666734946,-48.706329375));
#7631=CARTESIAN_POINT('Ctrl Pts',(24.3531646875,40.5208333401613,-42.1809185638422));
#7632=CARTESIAN_POINT('Ctrl Pts',(35.6555077526845,40.312500006828,-35.6555077526845));
#7633=CARTESIAN_POINT('Ctrl Pts',(42.1809185638422,40.1041666734946,-24.3531646875));
#7634=CARTESIAN_POINT('Ctrl Pts',(48.706329375,39.8958333401613,-13.0508216223155));
#7635=CARTESIAN_POINT('Ctrl Pts',(48.706329375,39.687500006828,1.293339198242E-14));
#7636=CARTESIAN_POINT('Ctrl Pts',(48.706329375,39.4791666734946,13.0508216223155));
#7637=CARTESIAN_POINT('Ctrl Pts',(42.1809185638422,39.2708333401613,24.3531646875));
#7638=CARTESIAN_POINT('Ctrl Pts',(35.6555077526845,39.062500006828,35.6555077526845));
#7639=CARTESIAN_POINT('Ctrl Pts',(24.3531646875,38.8541666734946,42.1809185638422));
#7640=CARTESIAN_POINT('Ctrl Pts',(13.0508216223155,38.6458333401613,48.706329375));
#7641=CARTESIAN_POINT('Ctrl Pts',(-9.95098946405443E-15,38.437500006828,
48.706329375));
#7642=CARTESIAN_POINT('Ctrl Pts',(-13.0508216223155,38.2291666734946,48.706329375));
#7643=CARTESIAN_POINT('Ctrl Pts',(-24.3531646875,38.0208333401613,42.1809185638423));
#7644=CARTESIAN_POINT('Ctrl Pts',(-35.6555077526845,37.812500006828,35.6555077526845));
#7645=CARTESIAN_POINT('Ctrl Pts',(-42.1809185638422,37.6041666734946,24.3531646875));
#7646=CARTESIAN_POINT('Ctrl Pts',(-48.706329375,37.3958333401613,13.0508216223155));
#7647=CARTESIAN_POINT('Ctrl Pts',(-48.706329375,37.187500006828,-1.8898197019151E-14));
#7648=CARTESIAN_POINT('Ctrl Pts',(-48.706329375,36.9791666734946,-13.0508216223155));
#7649=CARTESIAN_POINT('Ctrl Pts',(-42.1809185638422,36.7708333401613,-24.3531646875));
#7650=CARTESIAN_POINT('Ctrl Pts',(-35.6555077526845,36.562500006828,-35.6555077526845));
#7651=CARTESIAN_POINT('Ctrl Pts',(-24.3531646875,36.3541666734946,-42.1809185638423));
#7652=CARTESIAN_POINT('Ctrl Pts',(-13.0508216223155,36.1458333401613,-48.706329375));
#7653=CARTESIAN_POINT('Ctrl Pts',(1.59157945007855E-14,35.937500006828,
-48.706329375));
#7654=CARTESIAN_POINT('Ctrl Pts',(13.0508216223155,35.7291666734946,-48.706329375));
#7655=CARTESIAN_POINT('Ctrl Pts',(24.3531646875,35.5208333401613,-42.1809185638422));
#7656=CARTESIAN_POINT('Ctrl Pts',(35.6555077526845,35.312500006828,-35.6555077526845));
#7657=CARTESIAN_POINT('Ctrl Pts',(42.1809185638422,35.1041666734946,-24.3531646875));
#7658=CARTESIAN_POINT('Ctrl Pts',(48.706329375,34.8958333401613,-13.0508216223155));
#7659=CARTESIAN_POINT('Ctrl Pts',(48.706329375,34.687500006828,1.293339198242E-14));
#7660=CARTESIAN_POINT('Ctrl Pts',(48.706329375,34.4791666734946,13.0508216223155));
#7661=CARTESIAN_POINT('Ctrl Pts',(42.1809185638422,34.2708333401613,24.3531646875));
#7662=CARTESIAN_POINT('Ctrl Pts',(35.6555077526845,34.062500006828,35.6555077526845));
#7663=CARTESIAN_POINT('Ctrl Pts',(24.3531646875,33.8541666734946,42.1809185638422));
#7664=CARTESIAN_POINT('Ctrl Pts',(13.0508216223155,33.6458333401613,48.706329375));
#7665=CARTESIAN_POINT('Ctrl Pts',(-9.95098946405443E-15,33.437500006828,
48.706329375));
#7666=CARTESIAN_POINT('Ctrl Pts',(-13.0508216223155,33.2291666734946,48.706329375));
#7667=CARTESIAN_POINT('Ctrl Pts',(-24.3531646875,33.0208333401613,42.1809185638423));
#7668=CARTESIAN_POINT('Ctrl Pts',(-35.6555077526845,32.812500006828,35.6555077526845));
#7669=CARTESIAN_POINT('Ctrl Pts',(-42.1809185638422,32.6041666734946,24.3531646875));
#7670=CARTESIAN_POINT('Ctrl Pts',(-48.706329375,32.3958333401613,13.0508216223155));
#7671=CARTESIAN_POINT('Ctrl Pts',(-48.706329375,32.187500006828,-1.8898197019151E-14));
#7672=CARTESIAN_POINT('Ctrl Pts',(-48.706329375,31.9791666734946,-13.0508216223155));
#7673=CARTESIAN_POINT('Ctrl Pts',(-42.1809185638422,31.7708333401613,-24.3531646875));
#7674=CARTESIAN_POINT('Ctrl Pts',(-35.6555077526845,31.562500006828,-35.6555077526845));
#7675=CARTESIAN_POINT('Ctrl Pts',(-24.3531646875,31.3541666734946,-42.1809185638423));
#7676=CARTESIAN_POINT('Ctrl Pts',(-13.0508216223155,31.1458333401613,-48.706329375));
#7677=CARTESIAN_POINT('Ctrl Pts',(1.59157945007855E-14,30.937500006828,
-48.706329375));
#7678=CARTESIAN_POINT('Ctrl Pts',(13.0508216223155,30.7291666734946,-48.706329375));
#7679=CARTESIAN_POINT('Ctrl Pts',(24.3531646875,30.5208333401613,-42.1809185638422));
#7680=CARTESIAN_POINT('Ctrl Pts',(35.6555077526845,30.312500006828,-35.6555077526845));
#7681=CARTESIAN_POINT('Ctrl Pts',(42.1809185638422,30.1041666734946,-24.3531646875));
#7682=CARTESIAN_POINT('Ctrl Pts',(48.706329375,29.8958333401613,-13.0508216223155));
#7683=CARTESIAN_POINT('Ctrl Pts',(48.706329375,29.687500006828,1.293339198242E-14));
#7684=CARTESIAN_POINT('Ctrl Pts',(48.706329375,29.4791666734946,13.0508216223155));
#7685=CARTESIAN_POINT('Ctrl Pts',(42.1809185638422,29.2708333401613,24.3531646875));
#7686=CARTESIAN_POINT('Ctrl Pts',(35.6555077526845,29.062500006828,35.6555077526845));
#7687=CARTESIAN_POINT('Ctrl Pts',(24.3531646875,28.8541666734946,42.1809185638422));
#7688=CARTESIAN_POINT('Ctrl Pts',(13.0508216223155,28.6458333401613,48.706329375));
#7689=CARTESIAN_POINT('Ctrl Pts',(-9.95098946405443E-15,28.437500006828,
48.706329375));
#7690=CARTESIAN_POINT('Ctrl Pts',(-13.0508216223155,28.2291666734946,48.706329375));
#7691=CARTESIAN_POINT('Ctrl Pts',(-24.3531646875,28.0208333401613,42.1809185638423));
#7692=CARTESIAN_POINT('Ctrl Pts',(-35.6555077526845,27.812500006828,35.6555077526845));
#7693=CARTESIAN_POINT('Ctrl Pts',(-42.1809185638422,27.6041666734946,24.3531646875));
#7694=CARTESIAN_POINT('Ctrl Pts',(-48.706329375,27.3958333401613,13.0508216223155));
#7695=CARTESIAN_POINT('Ctrl Pts',(-48.706329375,27.187500006828,-1.8898197019151E-14));
#7696=CARTESIAN_POINT('',(3.61292728433798,40.8792520480093,-48.5721450795008));
#7697=CARTESIAN_POINT('',(48.5134353784345,39.7574536451604,-4.33048599679679));
#7698=CARTESIAN_POINT('Ctrl Pts',(3.61292728433798,40.8792520480092,-48.5721450795008));
#7699=CARTESIAN_POINT('Ctrl Pts',(14.7133549689477,40.6985216017706,-47.7464652997852));
#7700=CARTESIAN_POINT('Ctrl Pts',(24.3531646875,40.5208333401613,-42.1809185638422));
#7701=CARTESIAN_POINT('Ctrl Pts',(35.6555077526845,40.312500006828,-35.6555077526845));
#7702=CARTESIAN_POINT('Ctrl Pts',(42.1809185638422,40.1041666734946,-24.3531646875));
#7703=CARTESIAN_POINT('Ctrl Pts',(47.5573898704235,39.9325149229327,-15.0408432190651));
#7704=CARTESIAN_POINT('Ctrl Pts',(48.5134353784345,39.7574536451604,-4.33048599679679));
#7705=CARTESIAN_POINT('Origin',(-4513.80899746256,7993.28354997889,-4.33049059987538));
#7706=CARTESIAN_POINT('Ctrl Pts',(3.61292728433799,39.3132892765089,-45.8578974271399));
#7707=CARTESIAN_POINT('Ctrl Pts',(3.61292728433795,39.4468822859549,-46.089460636719));
#7708=CARTESIAN_POINT('Ctrl Pts',(3.61292728433823,39.7140705280013,-46.5525857733052));
#7709=CARTESIAN_POINT('Ctrl Pts',(3.61292728433805,39.9812630238615,-47.0157084557285));
#7710=CARTESIAN_POINT('Ctrl Pts',(3.61292728433805,40.3696539378594,-47.6888965792834));
#7711=CARTESIAN_POINT('Ctrl Pts',(3.61292728433798,40.624451287085,-48.1305218136162));
#7712=CARTESIAN_POINT('Ctrl Pts',(3.61292728433798,40.8792520480093,-48.5721450795008));
#7713=CARTESIAN_POINT('Ctrl Pts',(-46.,55.6250000136559,0.));
#7714=CARTESIAN_POINT('Ctrl Pts',(-46.,55.4166666803226,-12.3256628518316));
#7715=CARTESIAN_POINT('Ctrl Pts',(-39.8371685740842,55.2083333469893,-23.));
#7716=CARTESIAN_POINT('Ctrl Pts',(-33.6743371481684,55.0000000136559,-33.6743371481684));
#7717=CARTESIAN_POINT('Ctrl Pts',(-23.,54.7916666803226,-39.8371685740842));
#7718=CARTESIAN_POINT('Ctrl Pts',(-12.3256628518317,54.5833333469893,-46.));
#7719=CARTESIAN_POINT('Ctrl Pts',(-2.81668763803891E-15,54.3750000136559,
-46.));
#7720=CARTESIAN_POINT('Ctrl Pts',(12.3256628518316,54.1666666803226,-46.));
#7721=CARTESIAN_POINT('Ctrl Pts',(23.,53.9583333469893,-39.8371685740842));
#7722=CARTESIAN_POINT('Ctrl Pts',(33.6743371481683,53.7500000136559,-33.6743371481684));
#7723=CARTESIAN_POINT('Ctrl Pts',(39.8371685740842,53.5416666803226,-23.));
#7724=CARTESIAN_POINT('Ctrl Pts',(46.,53.3333333469893,-12.3256628518317));
#7725=CARTESIAN_POINT('Ctrl Pts',(46.,53.1250000136559,-5.63337527607782E-15));
#7726=CARTESIAN_POINT('Ctrl Pts',(46.,52.9166666803226,12.3256628518316));
#7727=CARTESIAN_POINT('Ctrl Pts',(39.8371685740842,52.7083333469893,23.));
#7728=CARTESIAN_POINT('Ctrl Pts',(33.6743371481684,52.5000000136559,33.6743371481683));
#7729=CARTESIAN_POINT('Ctrl Pts',(23.,52.2916666803226,39.8371685740842));
#7730=CARTESIAN_POINT('Ctrl Pts',(12.3256628518317,52.0833333469893,46.));
#7731=CARTESIAN_POINT('Ctrl Pts',(8.45006291411674E-15,51.8750000136559,
46.));
#7732=CARTESIAN_POINT('Ctrl Pts',(-12.3256628518316,51.6666666803226,46.));
#7733=CARTESIAN_POINT('Ctrl Pts',(-23.,51.4583333469893,39.8371685740842));
#7734=CARTESIAN_POINT('Ctrl Pts',(-33.6743371481683,51.2500000136559,33.6743371481684));
#7735=CARTESIAN_POINT('Ctrl Pts',(-39.8371685740842,51.0416666803226,23.));
#7736=CARTESIAN_POINT('Ctrl Pts',(-46.,50.8333333469893,12.3256628518317));
#7737=CARTESIAN_POINT('Ctrl Pts',(-46.,50.6250000136559,0.));
#7738=CARTESIAN_POINT('Ctrl Pts',(-46.,50.4166666803226,-12.3256628518316));
#7739=CARTESIAN_POINT('Ctrl Pts',(-39.8371685740842,50.2083333469893,-23.));
#7740=CARTESIAN_POINT('Ctrl Pts',(-33.6743371481684,50.0000000136559,-33.6743371481684));
#7741=CARTESIAN_POINT('Ctrl Pts',(-23.,49.7916666803226,-39.8371685740842));
#7742=CARTESIAN_POINT('Ctrl Pts',(-12.3256628518317,49.5833333469893,-46.));
#7743=CARTESIAN_POINT('Ctrl Pts',(-2.81668763803891E-15,49.3750000136559,
-46.));
#7744=CARTESIAN_POINT('Ctrl Pts',(12.3256628518316,49.1666666803226,-46.));
#7745=CARTESIAN_POINT('Ctrl Pts',(23.,48.9583333469893,-39.8371685740842));
#7746=CARTESIAN_POINT('Ctrl Pts',(33.6743371481683,48.7500000136559,-33.6743371481684));
#7747=CARTESIAN_POINT('Ctrl Pts',(39.8371685740842,48.5416666803226,-23.));
#7748=CARTESIAN_POINT('Ctrl Pts',(46.,48.3333333469893,-12.3256628518317));
#7749=CARTESIAN_POINT('Ctrl Pts',(46.,48.1250000136559,-5.63337527607782E-15));
#7750=CARTESIAN_POINT('Ctrl Pts',(46.,47.9166666803226,12.3256628518316));
#7751=CARTESIAN_POINT('Ctrl Pts',(39.8371685740842,47.7083333469893,23.));
#7752=CARTESIAN_POINT('Ctrl Pts',(33.6743371481684,47.5000000136559,33.6743371481683));
#7753=CARTESIAN_POINT('Ctrl Pts',(23.,47.2916666803226,39.8371685740842));
#7754=CARTESIAN_POINT('Ctrl Pts',(12.3256628518317,47.0833333469893,46.));
#7755=CARTESIAN_POINT('Ctrl Pts',(8.45006291411674E-15,46.8750000136559,
46.));
#7756=CARTESIAN_POINT('Ctrl Pts',(-12.3256628518316,46.6666666803226,46.));
#7757=CARTESIAN_POINT('Ctrl Pts',(-23.,46.4583333469893,39.8371685740842));
#7758=CARTESIAN_POINT('Ctrl Pts',(-33.6743371481683,46.2500000136559,33.6743371481684));
#7759=CARTESIAN_POINT('Ctrl Pts',(-39.8371685740842,46.0416666803226,23.));
#7760=CARTESIAN_POINT('Ctrl Pts',(-46.,45.8333333469892,12.3256628518317));
#7761=CARTESIAN_POINT('Ctrl Pts',(-46.,45.6250000136559,0.));
#7762=CARTESIAN_POINT('Ctrl Pts',(-46.,45.4166666803226,-12.3256628518316));
#7763=CARTESIAN_POINT('Ctrl Pts',(-39.8371685740842,45.2083333469893,-23.));
#7764=CARTESIAN_POINT('Ctrl Pts',(-33.6743371481684,45.0000000136559,-33.6743371481684));
#7765=CARTESIAN_POINT('Ctrl Pts',(-23.,44.7916666803226,-39.8371685740842));
#7766=CARTESIAN_POINT('Ctrl Pts',(-12.3256628518317,44.5833333469893,-46.));
#7767=CARTESIAN_POINT('Ctrl Pts',(-2.81668763803891E-15,44.3750000136559,
-46.));
#7768=CARTESIAN_POINT('Ctrl Pts',(12.3256628518316,44.1666666803226,-46.));
#7769=CARTESIAN_POINT('Ctrl Pts',(23.,43.9583333469893,-39.8371685740842));
#7770=CARTESIAN_POINT('Ctrl Pts',(33.6743371481683,43.7500000136559,-33.6743371481684));
#7771=CARTESIAN_POINT('Ctrl Pts',(39.8371685740842,43.5416666803226,-23.));
#7772=CARTESIAN_POINT('Ctrl Pts',(46.,43.3333333469893,-12.3256628518317));
#7773=CARTESIAN_POINT('Ctrl Pts',(46.,43.1250000136559,-5.63337527607782E-15));
#7774=CARTESIAN_POINT('Ctrl Pts',(46.,42.9166666803226,12.3256628518316));
#7775=CARTESIAN_POINT('Ctrl Pts',(39.8371685740842,42.7083333469893,23.));
#7776=CARTESIAN_POINT('Ctrl Pts',(33.6743371481684,42.5000000136559,33.6743371481683));
#7777=CARTESIAN_POINT('Ctrl Pts',(23.,42.2916666803226,39.8371685740842));
#7778=CARTESIAN_POINT('Ctrl Pts',(12.3256628518317,42.0833333469893,46.));
#7779=CARTESIAN_POINT('Ctrl Pts',(8.45006291411674E-15,41.8750000136559,
46.));
#7780=CARTESIAN_POINT('Ctrl Pts',(-12.3256628518316,41.6666666803226,46.));
#7781=CARTESIAN_POINT('Ctrl Pts',(-23.,41.4583333469893,39.8371685740842));
#7782=CARTESIAN_POINT('Ctrl Pts',(-33.6743371481683,41.2500000136559,33.6743371481684));
#7783=CARTESIAN_POINT('Ctrl Pts',(-39.8371685740842,41.0416666803226,23.));
#7784=CARTESIAN_POINT('Ctrl Pts',(-46.,40.8333333469893,12.3256628518317));
#7785=CARTESIAN_POINT('Ctrl Pts',(-46.,40.6250000136559,0.));
#7786=CARTESIAN_POINT('Ctrl Pts',(-46.,40.4166666803226,-12.3256628518316));
#7787=CARTESIAN_POINT('Ctrl Pts',(-39.8371685740842,40.2083333469893,-23.));
#7788=CARTESIAN_POINT('Ctrl Pts',(-33.6743371481684,40.0000000136559,-33.6743371481684));
#7789=CARTESIAN_POINT('Ctrl Pts',(-23.,39.7916666803226,-39.8371685740842));
#7790=CARTESIAN_POINT('Ctrl Pts',(-12.3256628518317,39.5833333469893,-46.));
#7791=CARTESIAN_POINT('Ctrl Pts',(-2.81668763803891E-15,39.3750000136559,
-46.));
#7792=CARTESIAN_POINT('Ctrl Pts',(12.3256628518316,39.1666666803226,-46.));
#7793=CARTESIAN_POINT('Ctrl Pts',(23.,38.9583333469893,-39.8371685740842));
#7794=CARTESIAN_POINT('Ctrl Pts',(33.6743371481683,38.7500000136559,-33.6743371481684));
#7795=CARTESIAN_POINT('Ctrl Pts',(39.8371685740842,38.5416666803226,-23.));
#7796=CARTESIAN_POINT('Ctrl Pts',(46.,38.3333333469893,-12.3256628518317));
#7797=CARTESIAN_POINT('Ctrl Pts',(46.,38.1250000136559,-5.63337527607782E-15));
#7798=CARTESIAN_POINT('Ctrl Pts',(46.,37.9166666803226,12.3256628518316));
#7799=CARTESIAN_POINT('Ctrl Pts',(39.8371685740842,37.7083333469893,23.));
#7800=CARTESIAN_POINT('Ctrl Pts',(33.6743371481684,37.5000000136559,33.6743371481683));
#7801=CARTESIAN_POINT('Ctrl Pts',(23.,37.2916666803226,39.8371685740842));
#7802=CARTESIAN_POINT('Ctrl Pts',(12.3256628518317,37.0833333469893,46.));
#7803=CARTESIAN_POINT('Ctrl Pts',(8.45006291411674E-15,36.8750000136559,
46.));
#7804=CARTESIAN_POINT('Ctrl Pts',(-12.3256628518316,36.6666666803226,46.));
#7805=CARTESIAN_POINT('Ctrl Pts',(-23.,36.4583333469893,39.8371685740842));
#7806=CARTESIAN_POINT('Ctrl Pts',(-33.6743371481683,36.2500000136559,33.6743371481684));
#7807=CARTESIAN_POINT('Ctrl Pts',(-39.8371685740842,36.0416666803226,23.));
#7808=CARTESIAN_POINT('Ctrl Pts',(-46.,35.8333333469893,12.3256628518317));
#7809=CARTESIAN_POINT('Ctrl Pts',(-46.,35.6250000136559,0.));
#7810=CARTESIAN_POINT('Ctrl Pts',(-46.,35.4166666803226,-12.3256628518316));
#7811=CARTESIAN_POINT('Ctrl Pts',(-39.8371685740842,35.2083333469893,-23.));
#7812=CARTESIAN_POINT('Ctrl Pts',(-33.6743371481684,35.0000000136559,-33.6743371481684));
#7813=CARTESIAN_POINT('Ctrl Pts',(-23.,34.7916666803226,-39.8371685740842));
#7814=CARTESIAN_POINT('Ctrl Pts',(-12.3256628518317,34.5833333469893,-46.));
#7815=CARTESIAN_POINT('Ctrl Pts',(-2.81668763803891E-15,34.3750000136559,
-46.));
#7816=CARTESIAN_POINT('Ctrl Pts',(12.3256628518316,34.1666666803226,-46.));
#7817=CARTESIAN_POINT('Ctrl Pts',(23.,33.9583333469893,-39.8371685740842));
#7818=CARTESIAN_POINT('Ctrl Pts',(33.6743371481683,33.7500000136559,-33.6743371481684));
#7819=CARTESIAN_POINT('Ctrl Pts',(39.8371685740842,33.5416666803226,-23.));
#7820=CARTESIAN_POINT('Ctrl Pts',(46.,33.3333333469893,-12.3256628518317));
#7821=CARTESIAN_POINT('Ctrl Pts',(46.,33.1250000136559,-5.63337527607782E-15));
#7822=CARTESIAN_POINT('Ctrl Pts',(46.,32.9166666803226,12.3256628518316));
#7823=CARTESIAN_POINT('Ctrl Pts',(39.8371685740842,32.7083333469893,23.));
#7824=CARTESIAN_POINT('Ctrl Pts',(33.6743371481684,32.5000000136559,33.6743371481683));
#7825=CARTESIAN_POINT('Ctrl Pts',(23.,32.2916666803226,39.8371685740842));
#7826=CARTESIAN_POINT('Ctrl Pts',(12.3256628518317,32.0833333469893,46.));
#7827=CARTESIAN_POINT('Ctrl Pts',(8.45006291411674E-15,31.8750000136559,
46.));
#7828=CARTESIAN_POINT('Ctrl Pts',(-12.3256628518316,31.6666666803226,46.));
#7829=CARTESIAN_POINT('Ctrl Pts',(-23.,31.4583333469893,39.8371685740842));
#7830=CARTESIAN_POINT('Ctrl Pts',(-33.6743371481683,31.2500000136559,33.6743371481684));
#7831=CARTESIAN_POINT('Ctrl Pts',(-39.8371685740842,31.0416666803226,23.));
#7832=CARTESIAN_POINT('Ctrl Pts',(-46.,30.8333333469893,12.3256628518317));
#7833=CARTESIAN_POINT('Ctrl Pts',(-46.,30.6250000136559,0.));
#7834=CARTESIAN_POINT('Ctrl Pts',(-46.,30.4166666803226,-12.3256628518316));
#7835=CARTESIAN_POINT('Ctrl Pts',(-39.8371685740842,30.2083333469893,-23.));
#7836=CARTESIAN_POINT('Ctrl Pts',(-33.6743371481684,30.0000000136559,-33.6743371481684));
#7837=CARTESIAN_POINT('Ctrl Pts',(-23.,29.7916666803226,-39.8371685740842));
#7838=CARTESIAN_POINT('Ctrl Pts',(-12.3256628518317,29.5833333469893,-46.));
#7839=CARTESIAN_POINT('Ctrl Pts',(-2.81668763803891E-15,29.3750000136559,
-46.));
#7840=CARTESIAN_POINT('Ctrl Pts',(12.3256628518316,29.1666666803226,-46.));
#7841=CARTESIAN_POINT('Ctrl Pts',(23.,28.9583333469893,-39.8371685740842));
#7842=CARTESIAN_POINT('Ctrl Pts',(33.6743371481683,28.7500000136559,-33.6743371481684));
#7843=CARTESIAN_POINT('Ctrl Pts',(39.8371685740842,28.5416666803226,-23.));
#7844=CARTESIAN_POINT('Ctrl Pts',(46.,28.3333333469893,-12.3256628518317));
#7845=CARTESIAN_POINT('Ctrl Pts',(46.,28.1250000136559,-5.63337527607782E-15));
#7846=CARTESIAN_POINT('Ctrl Pts',(46.,27.9166666803226,12.3256628518316));
#7847=CARTESIAN_POINT('Ctrl Pts',(39.8371685740842,27.7083333469893,23.));
#7848=CARTESIAN_POINT('Ctrl Pts',(33.6743371481684,27.5000000136559,33.6743371481683));
#7849=CARTESIAN_POINT('Ctrl Pts',(23.,27.2916666803226,39.8371685740842));
#7850=CARTESIAN_POINT('Ctrl Pts',(12.3256628518317,27.0833333469893,46.));
#7851=CARTESIAN_POINT('Ctrl Pts',(8.45006291411674E-15,26.8750000136559,
46.));
#7852=CARTESIAN_POINT('Ctrl Pts',(-12.3256628518316,26.6666666803226,46.));
#7853=CARTESIAN_POINT('Ctrl Pts',(-23.,26.4583333469893,39.8371685740842));
#7854=CARTESIAN_POINT('Ctrl Pts',(-33.6743371481683,26.2500000136559,33.6743371481684));
#7855=CARTESIAN_POINT('Ctrl Pts',(-39.8371685740842,26.0416666803226,23.));
#7856=CARTESIAN_POINT('Ctrl Pts',(-46.,25.8333333469893,12.3256628518317));
#7857=CARTESIAN_POINT('Ctrl Pts',(-46.,25.6250000136559,0.));
#7858=CARTESIAN_POINT('Ctrl Pts',(-48.706329375,57.187500006828,-1.8898197019151E-14));
#7859=CARTESIAN_POINT('Ctrl Pts',(-48.706329375,56.9791666734946,-13.0508216223155));
#7860=CARTESIAN_POINT('Ctrl Pts',(-42.1809185638422,56.7708333401613,-24.3531646875));
#7861=CARTESIAN_POINT('Ctrl Pts',(-35.6555077526845,56.562500006828,-35.6555077526845));
#7862=CARTESIAN_POINT('Ctrl Pts',(-24.3531646875,56.3541666734946,-42.1809185638423));
#7863=CARTESIAN_POINT('Ctrl Pts',(-13.0508216223155,56.1458333401613,-48.706329375));
#7864=CARTESIAN_POINT('Ctrl Pts',(1.59157945007855E-14,55.937500006828,
-48.706329375));
#7865=CARTESIAN_POINT('Ctrl Pts',(13.0508216223155,55.7291666734946,-48.706329375));
#7866=CARTESIAN_POINT('Ctrl Pts',(24.3531646875,55.5208333401613,-42.1809185638422));
#7867=CARTESIAN_POINT('Ctrl Pts',(35.6555077526845,55.312500006828,-35.6555077526845));
#7868=CARTESIAN_POINT('Ctrl Pts',(42.1809185638422,55.1041666734946,-24.3531646875));
#7869=CARTESIAN_POINT('Ctrl Pts',(48.706329375,54.8958333401613,-13.0508216223155));
#7870=CARTESIAN_POINT('Ctrl Pts',(48.706329375,54.687500006828,1.293339198242E-14));
#7871=CARTESIAN_POINT('Ctrl Pts',(48.706329375,54.4791666734946,13.0508216223155));
#7872=CARTESIAN_POINT('Ctrl Pts',(42.1809185638422,54.2708333401613,24.3531646875));
#7873=CARTESIAN_POINT('Ctrl Pts',(35.6555077526845,54.062500006828,35.6555077526845));
#7874=CARTESIAN_POINT('Ctrl Pts',(24.3531646875,53.8541666734946,42.1809185638422));
#7875=CARTESIAN_POINT('Ctrl Pts',(13.0508216223155,53.6458333401613,48.706329375));
#7876=CARTESIAN_POINT('Ctrl Pts',(-9.95098946405443E-15,53.437500006828,
48.706329375));
#7877=CARTESIAN_POINT('Ctrl Pts',(-13.0508216223155,53.2291666734946,48.706329375));
#7878=CARTESIAN_POINT('Ctrl Pts',(-24.3531646875,53.0208333401613,42.1809185638423));
#7879=CARTESIAN_POINT('Ctrl Pts',(-35.6555077526845,52.812500006828,35.6555077526845));
#7880=CARTESIAN_POINT('Ctrl Pts',(-42.1809185638422,52.6041666734946,24.3531646875));
#7881=CARTESIAN_POINT('Ctrl Pts',(-48.706329375,52.3958333401613,13.0508216223155));
#7882=CARTESIAN_POINT('Ctrl Pts',(-48.706329375,52.187500006828,-1.8898197019151E-14));
#7883=CARTESIAN_POINT('Ctrl Pts',(-48.706329375,51.9791666734946,-13.0508216223155));
#7884=CARTESIAN_POINT('Ctrl Pts',(-42.1809185638422,51.7708333401613,-24.3531646875));
#7885=CARTESIAN_POINT('Ctrl Pts',(-35.6555077526845,51.562500006828,-35.6555077526845));
#7886=CARTESIAN_POINT('Ctrl Pts',(-24.3531646875,51.3541666734946,-42.1809185638423));
#7887=CARTESIAN_POINT('Ctrl Pts',(-13.0508216223155,51.1458333401613,-48.706329375));
#7888=CARTESIAN_POINT('Ctrl Pts',(1.59157945007855E-14,50.937500006828,
-48.706329375));
#7889=CARTESIAN_POINT('Ctrl Pts',(13.0508216223155,50.7291666734946,-48.706329375));
#7890=CARTESIAN_POINT('Ctrl Pts',(24.3531646875,50.5208333401613,-42.1809185638422));
#7891=CARTESIAN_POINT('Ctrl Pts',(35.6555077526845,50.312500006828,-35.6555077526845));
#7892=CARTESIAN_POINT('Ctrl Pts',(42.1809185638422,50.1041666734946,-24.3531646875));
#7893=CARTESIAN_POINT('Ctrl Pts',(48.706329375,49.8958333401613,-13.0508216223155));
#7894=CARTESIAN_POINT('Ctrl Pts',(48.706329375,49.687500006828,1.293339198242E-14));
#7895=CARTESIAN_POINT('Ctrl Pts',(48.706329375,49.4791666734946,13.0508216223155));
#7896=CARTESIAN_POINT('Ctrl Pts',(42.1809185638422,49.2708333401613,24.3531646875));
#7897=CARTESIAN_POINT('Ctrl Pts',(35.6555077526845,49.062500006828,35.6555077526845));
#7898=CARTESIAN_POINT('Ctrl Pts',(24.3531646875,48.8541666734946,42.1809185638422));
#7899=CARTESIAN_POINT('Ctrl Pts',(13.0508216223155,48.6458333401613,48.706329375));
#7900=CARTESIAN_POINT('Ctrl Pts',(-9.95098946405443E-15,48.437500006828,
48.706329375));
#7901=CARTESIAN_POINT('Ctrl Pts',(-13.0508216223155,48.2291666734946,48.706329375));
#7902=CARTESIAN_POINT('Ctrl Pts',(-24.3531646875,48.0208333401613,42.1809185638423));
#7903=CARTESIAN_POINT('Ctrl Pts',(-35.6555077526845,47.812500006828,35.6555077526845));
#7904=CARTESIAN_POINT('Ctrl Pts',(-42.1809185638422,47.6041666734946,24.3531646875));
#7905=CARTESIAN_POINT('Ctrl Pts',(-48.706329375,47.3958333401613,13.0508216223155));
#7906=CARTESIAN_POINT('Ctrl Pts',(-48.706329375,47.187500006828,-1.8898197019151E-14));
#7907=CARTESIAN_POINT('Ctrl Pts',(-48.706329375,46.9791666734946,-13.0508216223155));
#7908=CARTESIAN_POINT('Ctrl Pts',(-42.1809185638422,46.7708333401613,-24.3531646875));
#7909=CARTESIAN_POINT('Ctrl Pts',(-35.6555077526845,46.562500006828,-35.6555077526845));
#7910=CARTESIAN_POINT('Ctrl Pts',(-24.3531646875,46.3541666734946,-42.1809185638423));
#7911=CARTESIAN_POINT('Ctrl Pts',(-13.0508216223155,46.1458333401613,-48.706329375));
#7912=CARTESIAN_POINT('Ctrl Pts',(1.59157945007855E-14,45.937500006828,
-48.706329375));
#7913=CARTESIAN_POINT('Ctrl Pts',(13.0508216223155,45.7291666734946,-48.706329375));
#7914=CARTESIAN_POINT('Ctrl Pts',(24.3531646875,45.5208333401613,-42.1809185638422));
#7915=CARTESIAN_POINT('Ctrl Pts',(35.6555077526845,45.312500006828,-35.6555077526845));
#7916=CARTESIAN_POINT('Ctrl Pts',(42.1809185638422,45.1041666734946,-24.3531646875));
#7917=CARTESIAN_POINT('Ctrl Pts',(48.706329375,44.8958333401613,-13.0508216223155));
#7918=CARTESIAN_POINT('Ctrl Pts',(48.706329375,44.687500006828,1.293339198242E-14));
#7919=CARTESIAN_POINT('Ctrl Pts',(48.706329375,44.4791666734946,13.0508216223155));
#7920=CARTESIAN_POINT('Ctrl Pts',(42.1809185638422,44.2708333401613,24.3531646875));
#7921=CARTESIAN_POINT('Ctrl Pts',(35.6555077526845,44.062500006828,35.6555077526845));
#7922=CARTESIAN_POINT('Ctrl Pts',(24.3531646875,43.8541666734946,42.1809185638422));
#7923=CARTESIAN_POINT('Ctrl Pts',(13.0508216223155,43.6458333401613,48.706329375));
#7924=CARTESIAN_POINT('Ctrl Pts',(-9.95098946405443E-15,43.437500006828,
48.706329375));
#7925=CARTESIAN_POINT('Ctrl Pts',(-13.0508216223155,43.2291666734946,48.706329375));
#7926=CARTESIAN_POINT('Ctrl Pts',(-24.3531646875,43.0208333401613,42.1809185638423));
#7927=CARTESIAN_POINT('Ctrl Pts',(-35.6555077526845,42.812500006828,35.6555077526845));
#7928=CARTESIAN_POINT('Ctrl Pts',(-42.1809185638422,42.6041666734946,24.3531646875));
#7929=CARTESIAN_POINT('Ctrl Pts',(-48.706329375,42.3958333401613,13.0508216223155));
#7930=CARTESIAN_POINT('Ctrl Pts',(-48.706329375,42.187500006828,-1.8898197019151E-14));
#7931=CARTESIAN_POINT('Ctrl Pts',(-48.706329375,41.9791666734946,-13.0508216223155));
#7932=CARTESIAN_POINT('Ctrl Pts',(-42.1809185638422,41.7708333401613,-24.3531646875));
#7933=CARTESIAN_POINT('Ctrl Pts',(-35.6555077526845,41.562500006828,-35.6555077526845));
#7934=CARTESIAN_POINT('Ctrl Pts',(-24.3531646875,41.3541666734946,-42.1809185638423));
#7935=CARTESIAN_POINT('Ctrl Pts',(-13.0508216223155,41.1458333401613,-48.706329375));
#7936=CARTESIAN_POINT('Ctrl Pts',(1.59157945007855E-14,40.937500006828,
-48.706329375));
#7937=CARTESIAN_POINT('Ctrl Pts',(13.0508216223155,40.7291666734946,-48.706329375));
#7938=CARTESIAN_POINT('Ctrl Pts',(24.3531646875,40.5208333401613,-42.1809185638422));
#7939=CARTESIAN_POINT('Ctrl Pts',(35.6555077526845,40.312500006828,-35.6555077526845));
#7940=CARTESIAN_POINT('Ctrl Pts',(42.1809185638422,40.1041666734946,-24.3531646875));
#7941=CARTESIAN_POINT('Ctrl Pts',(48.706329375,39.8958333401613,-13.0508216223155));
#7942=CARTESIAN_POINT('Ctrl Pts',(48.706329375,39.687500006828,1.293339198242E-14));
#7943=CARTESIAN_POINT('Ctrl Pts',(48.706329375,39.4791666734946,13.0508216223155));
#7944=CARTESIAN_POINT('Ctrl Pts',(42.1809185638422,39.2708333401613,24.3531646875));
#7945=CARTESIAN_POINT('Ctrl Pts',(35.6555077526845,39.062500006828,35.6555077526845));
#7946=CARTESIAN_POINT('Ctrl Pts',(24.3531646875,38.8541666734946,42.1809185638422));
#7947=CARTESIAN_POINT('Ctrl Pts',(13.0508216223155,38.6458333401613,48.706329375));
#7948=CARTESIAN_POINT('Ctrl Pts',(-9.95098946405443E-15,38.437500006828,
48.706329375));
#7949=CARTESIAN_POINT('Ctrl Pts',(-13.0508216223155,38.2291666734946,48.706329375));
#7950=CARTESIAN_POINT('Ctrl Pts',(-24.3531646875,38.0208333401613,42.1809185638423));
#7951=CARTESIAN_POINT('Ctrl Pts',(-35.6555077526845,37.812500006828,35.6555077526845));
#7952=CARTESIAN_POINT('Ctrl Pts',(-42.1809185638422,37.6041666734946,24.3531646875));
#7953=CARTESIAN_POINT('Ctrl Pts',(-48.706329375,37.3958333401613,13.0508216223155));
#7954=CARTESIAN_POINT('Ctrl Pts',(-48.706329375,37.187500006828,-1.8898197019151E-14));
#7955=CARTESIAN_POINT('Ctrl Pts',(-48.706329375,36.9791666734946,-13.0508216223155));
#7956=CARTESIAN_POINT('Ctrl Pts',(-42.1809185638422,36.7708333401613,-24.3531646875));
#7957=CARTESIAN_POINT('Ctrl Pts',(-35.6555077526845,36.562500006828,-35.6555077526845));
#7958=CARTESIAN_POINT('Ctrl Pts',(-24.3531646875,36.3541666734946,-42.1809185638423));
#7959=CARTESIAN_POINT('Ctrl Pts',(-13.0508216223155,36.1458333401613,-48.706329375));
#7960=CARTESIAN_POINT('Ctrl Pts',(1.59157945007855E-14,35.937500006828,
-48.706329375));
#7961=CARTESIAN_POINT('Ctrl Pts',(13.0508216223155,35.7291666734946,-48.706329375));
#7962=CARTESIAN_POINT('Ctrl Pts',(24.3531646875,35.5208333401613,-42.1809185638422));
#7963=CARTESIAN_POINT('Ctrl Pts',(35.6555077526845,35.312500006828,-35.6555077526845));
#7964=CARTESIAN_POINT('Ctrl Pts',(42.1809185638422,35.1041666734946,-24.3531646875));
#7965=CARTESIAN_POINT('Ctrl Pts',(48.706329375,34.8958333401613,-13.0508216223155));
#7966=CARTESIAN_POINT('Ctrl Pts',(48.706329375,34.687500006828,1.293339198242E-14));
#7967=CARTESIAN_POINT('Ctrl Pts',(48.706329375,34.4791666734946,13.0508216223155));
#7968=CARTESIAN_POINT('Ctrl Pts',(42.1809185638422,34.2708333401613,24.3531646875));
#7969=CARTESIAN_POINT('Ctrl Pts',(35.6555077526845,34.062500006828,35.6555077526845));
#7970=CARTESIAN_POINT('Ctrl Pts',(24.3531646875,33.8541666734946,42.1809185638422));
#7971=CARTESIAN_POINT('Ctrl Pts',(13.0508216223155,33.6458333401613,48.706329375));
#7972=CARTESIAN_POINT('Ctrl Pts',(-9.95098946405443E-15,33.437500006828,
48.706329375));
#7973=CARTESIAN_POINT('Ctrl Pts',(-13.0508216223155,33.2291666734946,48.706329375));
#7974=CARTESIAN_POINT('Ctrl Pts',(-24.3531646875,33.0208333401613,42.1809185638423));
#7975=CARTESIAN_POINT('Ctrl Pts',(-35.6555077526845,32.812500006828,35.6555077526845));
#7976=CARTESIAN_POINT('Ctrl Pts',(-42.1809185638422,32.6041666734946,24.3531646875));
#7977=CARTESIAN_POINT('Ctrl Pts',(-48.706329375,32.3958333401613,13.0508216223155));
#7978=CARTESIAN_POINT('Ctrl Pts',(-48.706329375,32.187500006828,-1.8898197019151E-14));
#7979=CARTESIAN_POINT('Ctrl Pts',(-48.706329375,31.9791666734946,-13.0508216223155));
#7980=CARTESIAN_POINT('Ctrl Pts',(-42.1809185638422,31.7708333401613,-24.3531646875));
#7981=CARTESIAN_POINT('Ctrl Pts',(-35.6555077526845,31.562500006828,-35.6555077526845));
#7982=CARTESIAN_POINT('Ctrl Pts',(-24.3531646875,31.3541666734946,-42.1809185638423));
#7983=CARTESIAN_POINT('Ctrl Pts',(-13.0508216223155,31.1458333401613,-48.706329375));
#7984=CARTESIAN_POINT('Ctrl Pts',(1.59157945007855E-14,30.937500006828,
-48.706329375));
#7985=CARTESIAN_POINT('Ctrl Pts',(13.0508216223155,30.7291666734946,-48.706329375));
#7986=CARTESIAN_POINT('Ctrl Pts',(24.3531646875,30.5208333401613,-42.1809185638422));
#7987=CARTESIAN_POINT('Ctrl Pts',(35.6555077526845,30.312500006828,-35.6555077526845));
#7988=CARTESIAN_POINT('Ctrl Pts',(42.1809185638422,30.1041666734946,-24.3531646875));
#7989=CARTESIAN_POINT('Ctrl Pts',(48.706329375,29.8958333401613,-13.0508216223155));
#7990=CARTESIAN_POINT('Ctrl Pts',(48.706329375,29.687500006828,1.293339198242E-14));
#7991=CARTESIAN_POINT('Ctrl Pts',(48.706329375,29.4791666734946,13.0508216223155));
#7992=CARTESIAN_POINT('Ctrl Pts',(42.1809185638422,29.2708333401613,24.3531646875));
#7993=CARTESIAN_POINT('Ctrl Pts',(35.6555077526845,29.062500006828,35.6555077526845));
#7994=CARTESIAN_POINT('Ctrl Pts',(24.3531646875,28.8541666734946,42.1809185638422));
#7995=CARTESIAN_POINT('Ctrl Pts',(13.0508216223155,28.6458333401613,48.706329375));
#7996=CARTESIAN_POINT('Ctrl Pts',(-9.95098946405443E-15,28.437500006828,
48.706329375));
#7997=CARTESIAN_POINT('Ctrl Pts',(-13.0508216223155,28.2291666734946,48.706329375));
#7998=CARTESIAN_POINT('Ctrl Pts',(-24.3531646875,28.0208333401613,42.1809185638423));
#7999=CARTESIAN_POINT('Ctrl Pts',(-35.6555077526845,27.812500006828,35.6555077526845));
#8000=CARTESIAN_POINT('Ctrl Pts',(-42.1809185638422,27.6041666734946,24.3531646875));
#8001=CARTESIAN_POINT('Ctrl Pts',(-48.706329375,27.3958333401613,13.0508216223155));
#8002=CARTESIAN_POINT('Ctrl Pts',(-48.706329375,27.187500006828,-1.8898197019151E-14));
#8003=CARTESIAN_POINT('',(48.5725845633798,39.6293483229262,3.60701400320329));
#8004=CARTESIAN_POINT('Ctrl Pts',(45.858362923034,38.0633913333999,3.60701400320327));
#8005=CARTESIAN_POINT('Ctrl Pts',(46.0899257719339,38.1969849680263,3.60701400320326));
#8006=CARTESIAN_POINT('Ctrl Pts',(46.5530501979845,38.4641744416604,3.60701400320347));
#8007=CARTESIAN_POINT('Ctrl Pts',(47.0161721905706,38.7313681332063,3.60701400320335));
#8008=CARTESIAN_POINT('Ctrl Pts',(47.6893519862319,39.1197565257476,3.60701400320335));
#8009=CARTESIAN_POINT('Ctrl Pts',(48.1309692507095,39.3745507329179,3.60701400320329));
#8010=CARTESIAN_POINT('Ctrl Pts',(48.5725845633798,39.6293483229262,3.60701400320329));
#8011=CARTESIAN_POINT('',(3.61292728433799,38.4957479656467,48.5721450795008));
#8012=CARTESIAN_POINT('Ctrl Pts',(48.5725845633798,39.6293483229262,3.60701400320329));
#8013=CARTESIAN_POINT('Ctrl Pts',(47.7480251419552,39.4485714020251,14.7106532430575));
#8014=CARTESIAN_POINT('Ctrl Pts',(42.1809185638422,39.2708333401613,24.3531646875));
#8015=CARTESIAN_POINT('Ctrl Pts',(35.6555077526845,39.062500006828,35.6555077526845));
#8016=CARTESIAN_POINT('Ctrl Pts',(24.3531646875,38.8541666734946,42.1809185638422));
#8017=CARTESIAN_POINT('Ctrl Pts',(14.7133549689477,38.6764784118853,47.7464652997852));
#8018=CARTESIAN_POINT('Ctrl Pts',(3.61292728433799,38.4957479656467,48.5721450795008));
#8019=CARTESIAN_POINT('',(3.61293045337837,36.9438035980764,45.8702489620438));
#8020=CARTESIAN_POINT('Ctrl Pts',(3.61292728433799,38.4957479656467,48.5721450795008));
#8021=CARTESIAN_POINT('Ctrl Pts',(3.61292728433799,38.3625660950884,48.3403451622817));
#8022=CARTESIAN_POINT('Ctrl Pts',(3.61292728433799,38.2293911846469,48.1085412459393));
#8023=CARTESIAN_POINT('Ctrl Pts',(3.61292728433799,38.0962235420553,47.8767331545518));
#8024=CARTESIAN_POINT('Ctrl Pts',(3.61292728433799,37.9630558994543,47.6449250631479));
#8025=CARTESIAN_POINT('Ctrl Pts',(3.61292728433799,37.8298955244832,47.4131127965212));
#8026=CARTESIAN_POINT('Ctrl Pts',(3.61292728433799,37.6967427432646,47.1812961682826));
#8027=CARTESIAN_POINT('Ctrl Pts',(3.61292728433799,37.4457351673773,46.7442964348035));
#8028=CARTESIAN_POINT('Ctrl Pts',(3.61292728433799,37.1947545598528,46.3072812097023));
#8029=CARTESIAN_POINT('Ctrl Pts',(3.61292728433799,36.9438035983105,45.8702489624514));
#8030=CARTESIAN_POINT('',(3.61293362241916,36.9438035983105,45.8702489624514));
#8031=CARTESIAN_POINT('Ctrl Pts',(-46.,55.6250000136559,0.));
#8032=CARTESIAN_POINT('Ctrl Pts',(-46.,55.4166666803226,-12.3256628518316));
#8033=CARTESIAN_POINT('Ctrl Pts',(-39.8371685740842,55.2083333469893,-23.));
#8034=CARTESIAN_POINT('Ctrl Pts',(-33.6743371481684,55.0000000136559,-33.6743371481684));
#8035=CARTESIAN_POINT('Ctrl Pts',(-23.,54.7916666803226,-39.8371685740842));
#8036=CARTESIAN_POINT('Ctrl Pts',(-12.3256628518317,54.5833333469893,-46.));
#8037=CARTESIAN_POINT('Ctrl Pts',(-2.81668763803891E-15,54.3750000136559,
-46.));
#8038=CARTESIAN_POINT('Ctrl Pts',(12.3256628518316,54.1666666803226,-46.));
#8039=CARTESIAN_POINT('Ctrl Pts',(23.,53.9583333469893,-39.8371685740842));
#8040=CARTESIAN_POINT('Ctrl Pts',(33.6743371481683,53.7500000136559,-33.6743371481684));
#8041=CARTESIAN_POINT('Ctrl Pts',(39.8371685740842,53.5416666803226,-23.));
#8042=CARTESIAN_POINT('Ctrl Pts',(46.,53.3333333469893,-12.3256628518317));
#8043=CARTESIAN_POINT('Ctrl Pts',(46.,53.1250000136559,-5.63337527607782E-15));
#8044=CARTESIAN_POINT('Ctrl Pts',(46.,52.9166666803226,12.3256628518316));
#8045=CARTESIAN_POINT('Ctrl Pts',(39.8371685740842,52.7083333469893,23.));
#8046=CARTESIAN_POINT('Ctrl Pts',(33.6743371481684,52.5000000136559,33.6743371481683));
#8047=CARTESIAN_POINT('Ctrl Pts',(23.,52.2916666803226,39.8371685740842));
#8048=CARTESIAN_POINT('Ctrl Pts',(12.3256628518317,52.0833333469893,46.));
#8049=CARTESIAN_POINT('Ctrl Pts',(8.45006291411674E-15,51.8750000136559,
46.));
#8050=CARTESIAN_POINT('Ctrl Pts',(-12.3256628518316,51.6666666803226,46.));
#8051=CARTESIAN_POINT('Ctrl Pts',(-23.,51.4583333469893,39.8371685740842));
#8052=CARTESIAN_POINT('Ctrl Pts',(-33.6743371481683,51.2500000136559,33.6743371481684));
#8053=CARTESIAN_POINT('Ctrl Pts',(-39.8371685740842,51.0416666803226,23.));
#8054=CARTESIAN_POINT('Ctrl Pts',(-46.,50.8333333469893,12.3256628518317));
#8055=CARTESIAN_POINT('Ctrl Pts',(-46.,50.6250000136559,0.));
#8056=CARTESIAN_POINT('Ctrl Pts',(-46.,50.4166666803226,-12.3256628518316));
#8057=CARTESIAN_POINT('Ctrl Pts',(-39.8371685740842,50.2083333469893,-23.));
#8058=CARTESIAN_POINT('Ctrl Pts',(-33.6743371481684,50.0000000136559,-33.6743371481684));
#8059=CARTESIAN_POINT('Ctrl Pts',(-23.,49.7916666803226,-39.8371685740842));
#8060=CARTESIAN_POINT('Ctrl Pts',(-12.3256628518317,49.5833333469893,-46.));
#8061=CARTESIAN_POINT('Ctrl Pts',(-2.81668763803891E-15,49.3750000136559,
-46.));
#8062=CARTESIAN_POINT('Ctrl Pts',(12.3256628518316,49.1666666803226,-46.));
#8063=CARTESIAN_POINT('Ctrl Pts',(23.,48.9583333469893,-39.8371685740842));
#8064=CARTESIAN_POINT('Ctrl Pts',(33.6743371481683,48.7500000136559,-33.6743371481684));
#8065=CARTESIAN_POINT('Ctrl Pts',(39.8371685740842,48.5416666803226,-23.));
#8066=CARTESIAN_POINT('Ctrl Pts',(46.,48.3333333469893,-12.3256628518317));
#8067=CARTESIAN_POINT('Ctrl Pts',(46.,48.1250000136559,-5.63337527607782E-15));
#8068=CARTESIAN_POINT('Ctrl Pts',(46.,47.9166666803226,12.3256628518316));
#8069=CARTESIAN_POINT('Ctrl Pts',(39.8371685740842,47.7083333469893,23.));
#8070=CARTESIAN_POINT('Ctrl Pts',(33.6743371481684,47.5000000136559,33.6743371481683));
#8071=CARTESIAN_POINT('Ctrl Pts',(23.,47.2916666803226,39.8371685740842));
#8072=CARTESIAN_POINT('Ctrl Pts',(12.3256628518317,47.0833333469893,46.));
#8073=CARTESIAN_POINT('Ctrl Pts',(8.45006291411674E-15,46.8750000136559,
46.));
#8074=CARTESIAN_POINT('Ctrl Pts',(-12.3256628518316,46.6666666803226,46.));
#8075=CARTESIAN_POINT('Ctrl Pts',(-23.,46.4583333469893,39.8371685740842));
#8076=CARTESIAN_POINT('Ctrl Pts',(-33.6743371481683,46.2500000136559,33.6743371481684));
#8077=CARTESIAN_POINT('Ctrl Pts',(-39.8371685740842,46.0416666803226,23.));
#8078=CARTESIAN_POINT('Ctrl Pts',(-46.,45.8333333469892,12.3256628518317));
#8079=CARTESIAN_POINT('Ctrl Pts',(-46.,45.6250000136559,0.));
#8080=CARTESIAN_POINT('Ctrl Pts',(-46.,45.4166666803226,-12.3256628518316));
#8081=CARTESIAN_POINT('Ctrl Pts',(-39.8371685740842,45.2083333469893,-23.));
#8082=CARTESIAN_POINT('Ctrl Pts',(-33.6743371481684,45.0000000136559,-33.6743371481684));
#8083=CARTESIAN_POINT('Ctrl Pts',(-23.,44.7916666803226,-39.8371685740842));
#8084=CARTESIAN_POINT('Ctrl Pts',(-12.3256628518317,44.5833333469893,-46.));
#8085=CARTESIAN_POINT('Ctrl Pts',(-2.81668763803891E-15,44.3750000136559,
-46.));
#8086=CARTESIAN_POINT('Ctrl Pts',(12.3256628518316,44.1666666803226,-46.));
#8087=CARTESIAN_POINT('Ctrl Pts',(23.,43.9583333469893,-39.8371685740842));
#8088=CARTESIAN_POINT('Ctrl Pts',(33.6743371481683,43.7500000136559,-33.6743371481684));
#8089=CARTESIAN_POINT('Ctrl Pts',(39.8371685740842,43.5416666803226,-23.));
#8090=CARTESIAN_POINT('Ctrl Pts',(46.,43.3333333469893,-12.3256628518317));
#8091=CARTESIAN_POINT('Ctrl Pts',(46.,43.1250000136559,-5.63337527607782E-15));
#8092=CARTESIAN_POINT('Ctrl Pts',(46.,42.9166666803226,12.3256628518316));
#8093=CARTESIAN_POINT('Ctrl Pts',(39.8371685740842,42.7083333469893,23.));
#8094=CARTESIAN_POINT('Ctrl Pts',(33.6743371481684,42.5000000136559,33.6743371481683));
#8095=CARTESIAN_POINT('Ctrl Pts',(23.,42.2916666803226,39.8371685740842));
#8096=CARTESIAN_POINT('Ctrl Pts',(12.3256628518317,42.0833333469893,46.));
#8097=CARTESIAN_POINT('Ctrl Pts',(8.45006291411674E-15,41.8750000136559,
46.));
#8098=CARTESIAN_POINT('Ctrl Pts',(-12.3256628518316,41.6666666803226,46.));
#8099=CARTESIAN_POINT('Ctrl Pts',(-23.,41.4583333469893,39.8371685740842));
#8100=CARTESIAN_POINT('Ctrl Pts',(-33.6743371481683,41.2500000136559,33.6743371481684));
#8101=CARTESIAN_POINT('Ctrl Pts',(-39.8371685740842,41.0416666803226,23.));
#8102=CARTESIAN_POINT('Ctrl Pts',(-46.,40.8333333469893,12.3256628518317));
#8103=CARTESIAN_POINT('Ctrl Pts',(-46.,40.6250000136559,0.));
#8104=CARTESIAN_POINT('Ctrl Pts',(-46.,40.4166666803226,-12.3256628518316));
#8105=CARTESIAN_POINT('Ctrl Pts',(-39.8371685740842,40.2083333469893,-23.));
#8106=CARTESIAN_POINT('Ctrl Pts',(-33.6743371481684,40.0000000136559,-33.6743371481684));
#8107=CARTESIAN_POINT('Ctrl Pts',(-23.,39.7916666803226,-39.8371685740842));
#8108=CARTESIAN_POINT('Ctrl Pts',(-12.3256628518317,39.5833333469893,-46.));
#8109=CARTESIAN_POINT('Ctrl Pts',(-2.81668763803891E-15,39.3750000136559,
-46.));
#8110=CARTESIAN_POINT('Ctrl Pts',(12.3256628518316,39.1666666803226,-46.));
#8111=CARTESIAN_POINT('Ctrl Pts',(23.,38.9583333469893,-39.8371685740842));
#8112=CARTESIAN_POINT('Ctrl Pts',(33.6743371481683,38.7500000136559,-33.6743371481684));
#8113=CARTESIAN_POINT('Ctrl Pts',(39.8371685740842,38.5416666803226,-23.));
#8114=CARTESIAN_POINT('Ctrl Pts',(46.,38.3333333469893,-12.3256628518317));
#8115=CARTESIAN_POINT('Ctrl Pts',(46.,38.1250000136559,-5.63337527607782E-15));
#8116=CARTESIAN_POINT('Ctrl Pts',(46.,37.9166666803226,12.3256628518316));
#8117=CARTESIAN_POINT('Ctrl Pts',(39.8371685740842,37.7083333469893,23.));
#8118=CARTESIAN_POINT('Ctrl Pts',(33.6743371481684,37.5000000136559,33.6743371481683));
#8119=CARTESIAN_POINT('Ctrl Pts',(23.,37.2916666803226,39.8371685740842));
#8120=CARTESIAN_POINT('Ctrl Pts',(12.3256628518317,37.0833333469893,46.));
#8121=CARTESIAN_POINT('Ctrl Pts',(8.45006291411674E-15,36.8750000136559,
46.));
#8122=CARTESIAN_POINT('Ctrl Pts',(-12.3256628518316,36.6666666803226,46.));
#8123=CARTESIAN_POINT('Ctrl Pts',(-23.,36.4583333469893,39.8371685740842));
#8124=CARTESIAN_POINT('Ctrl Pts',(-33.6743371481683,36.2500000136559,33.6743371481684));
#8125=CARTESIAN_POINT('Ctrl Pts',(-39.8371685740842,36.0416666803226,23.));
#8126=CARTESIAN_POINT('Ctrl Pts',(-46.,35.8333333469893,12.3256628518317));
#8127=CARTESIAN_POINT('Ctrl Pts',(-46.,35.6250000136559,0.));
#8128=CARTESIAN_POINT('Ctrl Pts',(-46.,35.4166666803226,-12.3256628518316));
#8129=CARTESIAN_POINT('Ctrl Pts',(-39.8371685740842,35.2083333469893,-23.));
#8130=CARTESIAN_POINT('Ctrl Pts',(-33.6743371481684,35.0000000136559,-33.6743371481684));
#8131=CARTESIAN_POINT('Ctrl Pts',(-23.,34.7916666803226,-39.8371685740842));
#8132=CARTESIAN_POINT('Ctrl Pts',(-12.3256628518317,34.5833333469893,-46.));
#8133=CARTESIAN_POINT('Ctrl Pts',(-2.81668763803891E-15,34.3750000136559,
-46.));
#8134=CARTESIAN_POINT('Ctrl Pts',(12.3256628518316,34.1666666803226,-46.));
#8135=CARTESIAN_POINT('Ctrl Pts',(23.,33.9583333469893,-39.8371685740842));
#8136=CARTESIAN_POINT('Ctrl Pts',(33.6743371481683,33.7500000136559,-33.6743371481684));
#8137=CARTESIAN_POINT('Ctrl Pts',(39.8371685740842,33.5416666803226,-23.));
#8138=CARTESIAN_POINT('Ctrl Pts',(46.,33.3333333469893,-12.3256628518317));
#8139=CARTESIAN_POINT('Ctrl Pts',(46.,33.1250000136559,-5.63337527607782E-15));
#8140=CARTESIAN_POINT('Ctrl Pts',(46.,32.9166666803226,12.3256628518316));
#8141=CARTESIAN_POINT('Ctrl Pts',(39.8371685740842,32.7083333469893,23.));
#8142=CARTESIAN_POINT('Ctrl Pts',(33.6743371481684,32.5000000136559,33.6743371481683));
#8143=CARTESIAN_POINT('Ctrl Pts',(23.,32.2916666803226,39.8371685740842));
#8144=CARTESIAN_POINT('Ctrl Pts',(12.3256628518317,32.0833333469893,46.));
#8145=CARTESIAN_POINT('Ctrl Pts',(8.45006291411674E-15,31.8750000136559,
46.));
#8146=CARTESIAN_POINT('Ctrl Pts',(-12.3256628518316,31.6666666803226,46.));
#8147=CARTESIAN_POINT('Ctrl Pts',(-23.,31.4583333469893,39.8371685740842));
#8148=CARTESIAN_POINT('Ctrl Pts',(-33.6743371481683,31.2500000136559,33.6743371481684));
#8149=CARTESIAN_POINT('Ctrl Pts',(-39.8371685740842,31.0416666803226,23.));
#8150=CARTESIAN_POINT('Ctrl Pts',(-46.,30.8333333469893,12.3256628518317));
#8151=CARTESIAN_POINT('Ctrl Pts',(-46.,30.6250000136559,0.));
#8152=CARTESIAN_POINT('Ctrl Pts',(-46.,30.4166666803226,-12.3256628518316));
#8153=CARTESIAN_POINT('Ctrl Pts',(-39.8371685740842,30.2083333469893,-23.));
#8154=CARTESIAN_POINT('Ctrl Pts',(-33.6743371481684,30.0000000136559,-33.6743371481684));
#8155=CARTESIAN_POINT('Ctrl Pts',(-23.,29.7916666803226,-39.8371685740842));
#8156=CARTESIAN_POINT('Ctrl Pts',(-12.3256628518317,29.5833333469893,-46.));
#8157=CARTESIAN_POINT('Ctrl Pts',(-2.81668763803891E-15,29.3750000136559,
-46.));
#8158=CARTESIAN_POINT('Ctrl Pts',(12.3256628518316,29.1666666803226,-46.));
#8159=CARTESIAN_POINT('Ctrl Pts',(23.,28.9583333469893,-39.8371685740842));
#8160=CARTESIAN_POINT('Ctrl Pts',(33.6743371481683,28.7500000136559,-33.6743371481684));
#8161=CARTESIAN_POINT('Ctrl Pts',(39.8371685740842,28.5416666803226,-23.));
#8162=CARTESIAN_POINT('Ctrl Pts',(46.,28.3333333469893,-12.3256628518317));
#8163=CARTESIAN_POINT('Ctrl Pts',(46.,28.1250000136559,-5.63337527607782E-15));
#8164=CARTESIAN_POINT('Ctrl Pts',(46.,27.9166666803226,12.3256628518316));
#8165=CARTESIAN_POINT('Ctrl Pts',(39.8371685740842,27.7083333469893,23.));
#8166=CARTESIAN_POINT('Ctrl Pts',(33.6743371481684,27.5000000136559,33.6743371481683));
#8167=CARTESIAN_POINT('Ctrl Pts',(23.,27.2916666803226,39.8371685740842));
#8168=CARTESIAN_POINT('Ctrl Pts',(12.3256628518317,27.0833333469893,46.));
#8169=CARTESIAN_POINT('Ctrl Pts',(8.45006291411674E-15,26.8750000136559,
46.));
#8170=CARTESIAN_POINT('Ctrl Pts',(-12.3256628518316,26.6666666803226,46.));
#8171=CARTESIAN_POINT('Ctrl Pts',(-23.,26.4583333469893,39.8371685740842));
#8172=CARTESIAN_POINT('Ctrl Pts',(-33.6743371481683,26.2500000136559,33.6743371481684));
#8173=CARTESIAN_POINT('Ctrl Pts',(-39.8371685740842,26.0416666803226,23.));
#8174=CARTESIAN_POINT('Ctrl Pts',(-46.,25.8333333469893,12.3256628518317));
#8175=CARTESIAN_POINT('Ctrl Pts',(-46.,25.6250000136559,0.));
#8176=CARTESIAN_POINT('Ctrl Pts',(-48.706329375,57.187500006828,-1.8898197019151E-14));
#8177=CARTESIAN_POINT('Ctrl Pts',(-48.706329375,56.9791666734946,-13.0508216223155));
#8178=CARTESIAN_POINT('Ctrl Pts',(-42.1809185638422,56.7708333401613,-24.3531646875));
#8179=CARTESIAN_POINT('Ctrl Pts',(-35.6555077526845,56.562500006828,-35.6555077526845));
#8180=CARTESIAN_POINT('Ctrl Pts',(-24.3531646875,56.3541666734946,-42.1809185638423));
#8181=CARTESIAN_POINT('Ctrl Pts',(-13.0508216223155,56.1458333401613,-48.706329375));
#8182=CARTESIAN_POINT('Ctrl Pts',(1.59157945007855E-14,55.937500006828,
-48.706329375));
#8183=CARTESIAN_POINT('Ctrl Pts',(13.0508216223155,55.7291666734946,-48.706329375));
#8184=CARTESIAN_POINT('Ctrl Pts',(24.3531646875,55.5208333401613,-42.1809185638422));
#8185=CARTESIAN_POINT('Ctrl Pts',(35.6555077526845,55.312500006828,-35.6555077526845));
#8186=CARTESIAN_POINT('Ctrl Pts',(42.1809185638422,55.1041666734946,-24.3531646875));
#8187=CARTESIAN_POINT('Ctrl Pts',(48.706329375,54.8958333401613,-13.0508216223155));
#8188=CARTESIAN_POINT('Ctrl Pts',(48.706329375,54.687500006828,1.293339198242E-14));
#8189=CARTESIAN_POINT('Ctrl Pts',(48.706329375,54.4791666734946,13.0508216223155));
#8190=CARTESIAN_POINT('Ctrl Pts',(42.1809185638422,54.2708333401613,24.3531646875));
#8191=CARTESIAN_POINT('Ctrl Pts',(35.6555077526845,54.062500006828,35.6555077526845));
#8192=CARTESIAN_POINT('Ctrl Pts',(24.3531646875,53.8541666734946,42.1809185638422));
#8193=CARTESIAN_POINT('Ctrl Pts',(13.0508216223155,53.6458333401613,48.706329375));
#8194=CARTESIAN_POINT('Ctrl Pts',(-9.95098946405443E-15,53.437500006828,
48.706329375));
#8195=CARTESIAN_POINT('Ctrl Pts',(-13.0508216223155,53.2291666734946,48.706329375));
#8196=CARTESIAN_POINT('Ctrl Pts',(-24.3531646875,53.0208333401613,42.1809185638423));
#8197=CARTESIAN_POINT('Ctrl Pts',(-35.6555077526845,52.812500006828,35.6555077526845));
#8198=CARTESIAN_POINT('Ctrl Pts',(-42.1809185638422,52.6041666734946,24.3531646875));
#8199=CARTESIAN_POINT('Ctrl Pts',(-48.706329375,52.3958333401613,13.0508216223155));
#8200=CARTESIAN_POINT('Ctrl Pts',(-48.706329375,52.187500006828,-1.8898197019151E-14));
#8201=CARTESIAN_POINT('Ctrl Pts',(-48.706329375,51.9791666734946,-13.0508216223155));
#8202=CARTESIAN_POINT('Ctrl Pts',(-42.1809185638422,51.7708333401613,-24.3531646875));
#8203=CARTESIAN_POINT('Ctrl Pts',(-35.6555077526845,51.562500006828,-35.6555077526845));
#8204=CARTESIAN_POINT('Ctrl Pts',(-24.3531646875,51.3541666734946,-42.1809185638423));
#8205=CARTESIAN_POINT('Ctrl Pts',(-13.0508216223155,51.1458333401613,-48.706329375));
#8206=CARTESIAN_POINT('Ctrl Pts',(1.59157945007855E-14,50.937500006828,
-48.706329375));
#8207=CARTESIAN_POINT('Ctrl Pts',(13.0508216223155,50.7291666734946,-48.706329375));
#8208=CARTESIAN_POINT('Ctrl Pts',(24.3531646875,50.5208333401613,-42.1809185638422));
#8209=CARTESIAN_POINT('Ctrl Pts',(35.6555077526845,50.312500006828,-35.6555077526845));
#8210=CARTESIAN_POINT('Ctrl Pts',(42.1809185638422,50.1041666734946,-24.3531646875));
#8211=CARTESIAN_POINT('Ctrl Pts',(48.706329375,49.8958333401613,-13.0508216223155));
#8212=CARTESIAN_POINT('Ctrl Pts',(48.706329375,49.687500006828,1.293339198242E-14));
#8213=CARTESIAN_POINT('Ctrl Pts',(48.706329375,49.4791666734946,13.0508216223155));
#8214=CARTESIAN_POINT('Ctrl Pts',(42.1809185638422,49.2708333401613,24.3531646875));
#8215=CARTESIAN_POINT('Ctrl Pts',(35.6555077526845,49.062500006828,35.6555077526845));
#8216=CARTESIAN_POINT('Ctrl Pts',(24.3531646875,48.8541666734946,42.1809185638422));
#8217=CARTESIAN_POINT('Ctrl Pts',(13.0508216223155,48.6458333401613,48.706329375));
#8218=CARTESIAN_POINT('Ctrl Pts',(-9.95098946405443E-15,48.437500006828,
48.706329375));
#8219=CARTESIAN_POINT('Ctrl Pts',(-13.0508216223155,48.2291666734946,48.706329375));
#8220=CARTESIAN_POINT('Ctrl Pts',(-24.3531646875,48.0208333401613,42.1809185638423));
#8221=CARTESIAN_POINT('Ctrl Pts',(-35.6555077526845,47.812500006828,35.6555077526845));
#8222=CARTESIAN_POINT('Ctrl Pts',(-42.1809185638422,47.6041666734946,24.3531646875));
#8223=CARTESIAN_POINT('Ctrl Pts',(-48.706329375,47.3958333401613,13.0508216223155));
#8224=CARTESIAN_POINT('Ctrl Pts',(-48.706329375,47.187500006828,-1.8898197019151E-14));
#8225=CARTESIAN_POINT('Ctrl Pts',(-48.706329375,46.9791666734946,-13.0508216223155));
#8226=CARTESIAN_POINT('Ctrl Pts',(-42.1809185638422,46.7708333401613,-24.3531646875));
#8227=CARTESIAN_POINT('Ctrl Pts',(-35.6555077526845,46.562500006828,-35.6555077526845));
#8228=CARTESIAN_POINT('Ctrl Pts',(-24.3531646875,46.3541666734946,-42.1809185638423));
#8229=CARTESIAN_POINT('Ctrl Pts',(-13.0508216223155,46.1458333401613,-48.706329375));
#8230=CARTESIAN_POINT('Ctrl Pts',(1.59157945007855E-14,45.937500006828,
-48.706329375));
#8231=CARTESIAN_POINT('Ctrl Pts',(13.0508216223155,45.7291666734946,-48.706329375));
#8232=CARTESIAN_POINT('Ctrl Pts',(24.3531646875,45.5208333401613,-42.1809185638422));
#8233=CARTESIAN_POINT('Ctrl Pts',(35.6555077526845,45.312500006828,-35.6555077526845));
#8234=CARTESIAN_POINT('Ctrl Pts',(42.1809185638422,45.1041666734946,-24.3531646875));
#8235=CARTESIAN_POINT('Ctrl Pts',(48.706329375,44.8958333401613,-13.0508216223155));
#8236=CARTESIAN_POINT('Ctrl Pts',(48.706329375,44.687500006828,1.293339198242E-14));
#8237=CARTESIAN_POINT('Ctrl Pts',(48.706329375,44.4791666734946,13.0508216223155));
#8238=CARTESIAN_POINT('Ctrl Pts',(42.1809185638422,44.2708333401613,24.3531646875));
#8239=CARTESIAN_POINT('Ctrl Pts',(35.6555077526845,44.062500006828,35.6555077526845));
#8240=CARTESIAN_POINT('Ctrl Pts',(24.3531646875,43.8541666734946,42.1809185638422));
#8241=CARTESIAN_POINT('Ctrl Pts',(13.0508216223155,43.6458333401613,48.706329375));
#8242=CARTESIAN_POINT('Ctrl Pts',(-9.95098946405443E-15,43.437500006828,
48.706329375));
#8243=CARTESIAN_POINT('Ctrl Pts',(-13.0508216223155,43.2291666734946,48.706329375));
#8244=CARTESIAN_POINT('Ctrl Pts',(-24.3531646875,43.0208333401613,42.1809185638423));
#8245=CARTESIAN_POINT('Ctrl Pts',(-35.6555077526845,42.812500006828,35.6555077526845));
#8246=CARTESIAN_POINT('Ctrl Pts',(-42.1809185638422,42.6041666734946,24.3531646875));
#8247=CARTESIAN_POINT('Ctrl Pts',(-48.706329375,42.3958333401613,13.0508216223155));
#8248=CARTESIAN_POINT('Ctrl Pts',(-48.706329375,42.187500006828,-1.8898197019151E-14));
#8249=CARTESIAN_POINT('Ctrl Pts',(-48.706329375,41.9791666734946,-13.0508216223155));
#8250=CARTESIAN_POINT('Ctrl Pts',(-42.1809185638422,41.7708333401613,-24.3531646875));
#8251=CARTESIAN_POINT('Ctrl Pts',(-35.6555077526845,41.562500006828,-35.6555077526845));
#8252=CARTESIAN_POINT('Ctrl Pts',(-24.3531646875,41.3541666734946,-42.1809185638423));
#8253=CARTESIAN_POINT('Ctrl Pts',(-13.0508216223155,41.1458333401613,-48.706329375));
#8254=CARTESIAN_POINT('Ctrl Pts',(1.59157945007855E-14,40.937500006828,
-48.706329375));
#8255=CARTESIAN_POINT('Ctrl Pts',(13.0508216223155,40.7291666734946,-48.706329375));
#8256=CARTESIAN_POINT('Ctrl Pts',(24.3531646875,40.5208333401613,-42.1809185638422));
#8257=CARTESIAN_POINT('Ctrl Pts',(35.6555077526845,40.312500006828,-35.6555077526845));
#8258=CARTESIAN_POINT('Ctrl Pts',(42.1809185638422,40.1041666734946,-24.3531646875));
#8259=CARTESIAN_POINT('Ctrl Pts',(48.706329375,39.8958333401613,-13.0508216223155));
#8260=CARTESIAN_POINT('Ctrl Pts',(48.706329375,39.687500006828,1.293339198242E-14));
#8261=CARTESIAN_POINT('Ctrl Pts',(48.706329375,39.4791666734946,13.0508216223155));
#8262=CARTESIAN_POINT('Ctrl Pts',(42.1809185638422,39.2708333401613,24.3531646875));
#8263=CARTESIAN_POINT('Ctrl Pts',(35.6555077526845,39.062500006828,35.6555077526845));
#8264=CARTESIAN_POINT('Ctrl Pts',(24.3531646875,38.8541666734946,42.1809185638422));
#8265=CARTESIAN_POINT('Ctrl Pts',(13.0508216223155,38.6458333401613,48.706329375));
#8266=CARTESIAN_POINT('Ctrl Pts',(-9.95098946405443E-15,38.437500006828,
48.706329375));
#8267=CARTESIAN_POINT('Ctrl Pts',(-13.0508216223155,38.2291666734946,48.706329375));
#8268=CARTESIAN_POINT('Ctrl Pts',(-24.3531646875,38.0208333401613,42.1809185638423));
#8269=CARTESIAN_POINT('Ctrl Pts',(-35.6555077526845,37.812500006828,35.6555077526845));
#8270=CARTESIAN_POINT('Ctrl Pts',(-42.1809185638422,37.6041666734946,24.3531646875));
#8271=CARTESIAN_POINT('Ctrl Pts',(-48.706329375,37.3958333401613,13.0508216223155));
#8272=CARTESIAN_POINT('Ctrl Pts',(-48.706329375,37.187500006828,-1.8898197019151E-14));
#8273=CARTESIAN_POINT('Ctrl Pts',(-48.706329375,36.9791666734946,-13.0508216223155));
#8274=CARTESIAN_POINT('Ctrl Pts',(-42.1809185638422,36.7708333401613,-24.3531646875));
#8275=CARTESIAN_POINT('Ctrl Pts',(-35.6555077526845,36.562500006828,-35.6555077526845));
#8276=CARTESIAN_POINT('Ctrl Pts',(-24.3531646875,36.3541666734946,-42.1809185638423));
#8277=CARTESIAN_POINT('Ctrl Pts',(-13.0508216223155,36.1458333401613,-48.706329375));
#8278=CARTESIAN_POINT('Ctrl Pts',(1.59157945007855E-14,35.937500006828,
-48.706329375));
#8279=CARTESIAN_POINT('Ctrl Pts',(13.0508216223155,35.7291666734946,-48.706329375));
#8280=CARTESIAN_POINT('Ctrl Pts',(24.3531646875,35.5208333401613,-42.1809185638422));
#8281=CARTESIAN_POINT('Ctrl Pts',(35.6555077526845,35.312500006828,-35.6555077526845));
#8282=CARTESIAN_POINT('Ctrl Pts',(42.1809185638422,35.1041666734946,-24.3531646875));
#8283=CARTESIAN_POINT('Ctrl Pts',(48.706329375,34.8958333401613,-13.0508216223155));
#8284=CARTESIAN_POINT('Ctrl Pts',(48.706329375,34.687500006828,1.293339198242E-14));
#8285=CARTESIAN_POINT('Ctrl Pts',(48.706329375,34.4791666734946,13.0508216223155));
#8286=CARTESIAN_POINT('Ctrl Pts',(42.1809185638422,34.2708333401613,24.3531646875));
#8287=CARTESIAN_POINT('Ctrl Pts',(35.6555077526845,34.062500006828,35.6555077526845));
#8288=CARTESIAN_POINT('Ctrl Pts',(24.3531646875,33.8541666734946,42.1809185638422));
#8289=CARTESIAN_POINT('Ctrl Pts',(13.0508216223155,33.6458333401613,48.706329375));
#8290=CARTESIAN_POINT('Ctrl Pts',(-9.95098946405443E-15,33.437500006828,
48.706329375));
#8291=CARTESIAN_POINT('Ctrl Pts',(-13.0508216223155,33.2291666734946,48.706329375));
#8292=CARTESIAN_POINT('Ctrl Pts',(-24.3531646875,33.0208333401613,42.1809185638423));
#8293=CARTESIAN_POINT('Ctrl Pts',(-35.6555077526845,32.812500006828,35.6555077526845));
#8294=CARTESIAN_POINT('Ctrl Pts',(-42.1809185638422,32.6041666734946,24.3531646875));
#8295=CARTESIAN_POINT('Ctrl Pts',(-48.706329375,32.3958333401613,13.0508216223155));
#8296=CARTESIAN_POINT('Ctrl Pts',(-48.706329375,32.187500006828,-1.8898197019151E-14));
#8297=CARTESIAN_POINT('Ctrl Pts',(-48.706329375,31.9791666734946,-13.0508216223155));
#8298=CARTESIAN_POINT('Ctrl Pts',(-42.1809185638422,31.7708333401613,-24.3531646875));
#8299=CARTESIAN_POINT('Ctrl Pts',(-35.6555077526845,31.562500006828,-35.6555077526845));
#8300=CARTESIAN_POINT('Ctrl Pts',(-24.3531646875,31.3541666734946,-42.1809185638423));
#8301=CARTESIAN_POINT('Ctrl Pts',(-13.0508216223155,31.1458333401613,-48.706329375));
#8302=CARTESIAN_POINT('Ctrl Pts',(1.59157945007855E-14,30.937500006828,
-48.706329375));
#8303=CARTESIAN_POINT('Ctrl Pts',(13.0508216223155,30.7291666734946,-48.706329375));
#8304=CARTESIAN_POINT('Ctrl Pts',(24.3531646875,30.5208333401613,-42.1809185638422));
#8305=CARTESIAN_POINT('Ctrl Pts',(35.6555077526845,30.312500006828,-35.6555077526845));
#8306=CARTESIAN_POINT('Ctrl Pts',(42.1809185638422,30.1041666734946,-24.3531646875));
#8307=CARTESIAN_POINT('Ctrl Pts',(48.706329375,29.8958333401613,-13.0508216223155));
#8308=CARTESIAN_POINT('Ctrl Pts',(48.706329375,29.687500006828,1.293339198242E-14));
#8309=CARTESIAN_POINT('Ctrl Pts',(48.706329375,29.4791666734946,13.0508216223155));
#8310=CARTESIAN_POINT('Ctrl Pts',(42.1809185638422,29.2708333401613,24.3531646875));
#8311=CARTESIAN_POINT('Ctrl Pts',(35.6555077526845,29.062500006828,35.6555077526845));
#8312=CARTESIAN_POINT('Ctrl Pts',(24.3531646875,28.8541666734946,42.1809185638422));
#8313=CARTESIAN_POINT('Ctrl Pts',(13.0508216223155,28.6458333401613,48.706329375));
#8314=CARTESIAN_POINT('Ctrl Pts',(-9.95098946405443E-15,28.437500006828,
48.706329375));
#8315=CARTESIAN_POINT('Ctrl Pts',(-13.0508216223155,28.2291666734946,48.706329375));
#8316=CARTESIAN_POINT('Ctrl Pts',(-24.3531646875,28.0208333401613,42.1809185638423));
#8317=CARTESIAN_POINT('Ctrl Pts',(-35.6555077526845,27.812500006828,35.6555077526845));
#8318=CARTESIAN_POINT('Ctrl Pts',(-42.1809185638422,27.6041666734946,24.3531646875));
#8319=CARTESIAN_POINT('Ctrl Pts',(-48.706329375,27.3958333401613,13.0508216223155));
#8320=CARTESIAN_POINT('Ctrl Pts',(-48.706329375,27.187500006828,-1.8898197019151E-14));
#8321=CARTESIAN_POINT('',(-48.3095415605567,56.9999999999858,-4.33048599679673));
#8322=CARTESIAN_POINT('Ctrl Pts',(-45.7957082162897,55.5508791552084,-4.33048599679673));
#8323=CARTESIAN_POINT('Ctrl Pts',(-46.027322302781,55.6843839384496,-4.33048599679673));
#8324=CARTESIAN_POINT('Ctrl Pts',(-46.4905476657728,55.9513983799647,-4.33048599679673));
#8325=CARTESIAN_POINT('Ctrl Pts',(-46.9537676533565,56.2184221466352,-4.33048599679673));
#8326=CARTESIAN_POINT('Ctrl Pts',(-47.5601013844768,56.5679517997618,-4.33048599679673));
#8327=CARTESIAN_POINT('Ctrl Pts',(-47.9348230422494,56.7839731770798,-4.33048599679673));
#8328=CARTESIAN_POINT('Ctrl Pts',(-48.3095415605567,56.9999999999858,-4.33048599679673));
#8329=CARTESIAN_POINT('',(-48.0678199532544,57.,-7.03922488851235));
#8330=CARTESIAN_POINT('Origin',(0.322758650769908,56.9999468614787,-1.35580654760172));
#8331=CARTESIAN_POINT('',(-48.3871149493437,57.0447214927916,-4.33048599679673));
#8332=CARTESIAN_POINT('Origin',(0.0124715173034229,56.9065257752989,0.00338253564322266));
#8333=CARTESIAN_POINT('',(-48.5134353784345,57.1175463684955,-4.33048599679673));
#8334=CARTESIAN_POINT('',(-48.3871149493437,57.0447214927916,-4.33048599679673));
#8335=CARTESIAN_POINT('',(-4.32456003949879,56.0073567866782,-48.5139639861634));
#8336=CARTESIAN_POINT('Ctrl Pts',(-48.5134353784344,57.1175463684955,-4.33048599679673));
#8337=CARTESIAN_POINT('Ctrl Pts',(-47.5573898704235,56.9424850907232,-15.0408432190651));
#8338=CARTESIAN_POINT('Ctrl Pts',(-42.1809185638422,56.7708333401613,-24.3531646875));
#8339=CARTESIAN_POINT('Ctrl Pts',(-35.6555077526845,56.562500006828,-35.6555077526845));
#8340=CARTESIAN_POINT('Ctrl Pts',(-24.3531646875,56.3541666734946,-42.1809185638423));
#8341=CARTESIAN_POINT('Ctrl Pts',(-15.038141415499,56.1824651212465,-47.5589497574396));
#8342=CARTESIAN_POINT('Ctrl Pts',(-4.32456003949879,56.0073567866783,-48.5139639861634));
#8343=CARTESIAN_POINT('Origin',(-4.32456007771086,8027.20453909234,4524.01087309897));
#8344=CARTESIAN_POINT('Ctrl Pts',(-46.,55.6250000136559,0.));
#8345=CARTESIAN_POINT('Ctrl Pts',(-46.,55.4166666803226,-12.3256628518316));
#8346=CARTESIAN_POINT('Ctrl Pts',(-39.8371685740842,55.2083333469893,-23.));
#8347=CARTESIAN_POINT('Ctrl Pts',(-33.6743371481684,55.0000000136559,-33.6743371481684));
#8348=CARTESIAN_POINT('Ctrl Pts',(-23.,54.7916666803226,-39.8371685740842));
#8349=CARTESIAN_POINT('Ctrl Pts',(-12.3256628518317,54.5833333469893,-46.));
#8350=CARTESIAN_POINT('Ctrl Pts',(-2.81668763803891E-15,54.3750000136559,
-46.));
#8351=CARTESIAN_POINT('Ctrl Pts',(12.3256628518316,54.1666666803226,-46.));
#8352=CARTESIAN_POINT('Ctrl Pts',(23.,53.9583333469893,-39.8371685740842));
#8353=CARTESIAN_POINT('Ctrl Pts',(33.6743371481683,53.7500000136559,-33.6743371481684));
#8354=CARTESIAN_POINT('Ctrl Pts',(39.8371685740842,53.5416666803226,-23.));
#8355=CARTESIAN_POINT('Ctrl Pts',(46.,53.3333333469893,-12.3256628518317));
#8356=CARTESIAN_POINT('Ctrl Pts',(46.,53.1250000136559,-5.63337527607782E-15));
#8357=CARTESIAN_POINT('Ctrl Pts',(46.,52.9166666803226,12.3256628518316));
#8358=CARTESIAN_POINT('Ctrl Pts',(39.8371685740842,52.7083333469893,23.));
#8359=CARTESIAN_POINT('Ctrl Pts',(33.6743371481684,52.5000000136559,33.6743371481683));
#8360=CARTESIAN_POINT('Ctrl Pts',(23.,52.2916666803226,39.8371685740842));
#8361=CARTESIAN_POINT('Ctrl Pts',(12.3256628518317,52.0833333469893,46.));
#8362=CARTESIAN_POINT('Ctrl Pts',(8.45006291411674E-15,51.8750000136559,
46.));
#8363=CARTESIAN_POINT('Ctrl Pts',(-12.3256628518316,51.6666666803226,46.));
#8364=CARTESIAN_POINT('Ctrl Pts',(-23.,51.4583333469893,39.8371685740842));
#8365=CARTESIAN_POINT('Ctrl Pts',(-33.6743371481683,51.2500000136559,33.6743371481684));
#8366=CARTESIAN_POINT('Ctrl Pts',(-39.8371685740842,51.0416666803226,23.));
#8367=CARTESIAN_POINT('Ctrl Pts',(-46.,50.8333333469893,12.3256628518317));
#8368=CARTESIAN_POINT('Ctrl Pts',(-46.,50.6250000136559,0.));
#8369=CARTESIAN_POINT('Ctrl Pts',(-46.,50.4166666803226,-12.3256628518316));
#8370=CARTESIAN_POINT('Ctrl Pts',(-39.8371685740842,50.2083333469893,-23.));
#8371=CARTESIAN_POINT('Ctrl Pts',(-33.6743371481684,50.0000000136559,-33.6743371481684));
#8372=CARTESIAN_POINT('Ctrl Pts',(-23.,49.7916666803226,-39.8371685740842));
#8373=CARTESIAN_POINT('Ctrl Pts',(-12.3256628518317,49.5833333469893,-46.));
#8374=CARTESIAN_POINT('Ctrl Pts',(-2.81668763803891E-15,49.3750000136559,
-46.));
#8375=CARTESIAN_POINT('Ctrl Pts',(12.3256628518316,49.1666666803226,-46.));
#8376=CARTESIAN_POINT('Ctrl Pts',(23.,48.9583333469893,-39.8371685740842));
#8377=CARTESIAN_POINT('Ctrl Pts',(33.6743371481683,48.7500000136559,-33.6743371481684));
#8378=CARTESIAN_POINT('Ctrl Pts',(39.8371685740842,48.5416666803226,-23.));
#8379=CARTESIAN_POINT('Ctrl Pts',(46.,48.3333333469893,-12.3256628518317));
#8380=CARTESIAN_POINT('Ctrl Pts',(46.,48.1250000136559,-5.63337527607782E-15));
#8381=CARTESIAN_POINT('Ctrl Pts',(46.,47.9166666803226,12.3256628518316));
#8382=CARTESIAN_POINT('Ctrl Pts',(39.8371685740842,47.7083333469893,23.));
#8383=CARTESIAN_POINT('Ctrl Pts',(33.6743371481684,47.5000000136559,33.6743371481683));
#8384=CARTESIAN_POINT('Ctrl Pts',(23.,47.2916666803226,39.8371685740842));
#8385=CARTESIAN_POINT('Ctrl Pts',(12.3256628518317,47.0833333469893,46.));
#8386=CARTESIAN_POINT('Ctrl Pts',(8.45006291411674E-15,46.8750000136559,
46.));
#8387=CARTESIAN_POINT('Ctrl Pts',(-12.3256628518316,46.6666666803226,46.));
#8388=CARTESIAN_POINT('Ctrl Pts',(-23.,46.4583333469893,39.8371685740842));
#8389=CARTESIAN_POINT('Ctrl Pts',(-33.6743371481683,46.2500000136559,33.6743371481684));
#8390=CARTESIAN_POINT('Ctrl Pts',(-39.8371685740842,46.0416666803226,23.));
#8391=CARTESIAN_POINT('Ctrl Pts',(-46.,45.8333333469892,12.3256628518317));
#8392=CARTESIAN_POINT('Ctrl Pts',(-46.,45.6250000136559,0.));
#8393=CARTESIAN_POINT('Ctrl Pts',(-46.,45.4166666803226,-12.3256628518316));
#8394=CARTESIAN_POINT('Ctrl Pts',(-39.8371685740842,45.2083333469893,-23.));
#8395=CARTESIAN_POINT('Ctrl Pts',(-33.6743371481684,45.0000000136559,-33.6743371481684));
#8396=CARTESIAN_POINT('Ctrl Pts',(-23.,44.7916666803226,-39.8371685740842));
#8397=CARTESIAN_POINT('Ctrl Pts',(-12.3256628518317,44.5833333469893,-46.));
#8398=CARTESIAN_POINT('Ctrl Pts',(-2.81668763803891E-15,44.3750000136559,
-46.));
#8399=CARTESIAN_POINT('Ctrl Pts',(12.3256628518316,44.1666666803226,-46.));
#8400=CARTESIAN_POINT('Ctrl Pts',(23.,43.9583333469893,-39.8371685740842));
#8401=CARTESIAN_POINT('Ctrl Pts',(33.6743371481683,43.7500000136559,-33.6743371481684));
#8402=CARTESIAN_POINT('Ctrl Pts',(39.8371685740842,43.5416666803226,-23.));
#8403=CARTESIAN_POINT('Ctrl Pts',(46.,43.3333333469893,-12.3256628518317));
#8404=CARTESIAN_POINT('Ctrl Pts',(46.,43.1250000136559,-5.63337527607782E-15));
#8405=CARTESIAN_POINT('Ctrl Pts',(46.,42.9166666803226,12.3256628518316));
#8406=CARTESIAN_POINT('Ctrl Pts',(39.8371685740842,42.7083333469893,23.));
#8407=CARTESIAN_POINT('Ctrl Pts',(33.6743371481684,42.5000000136559,33.6743371481683));
#8408=CARTESIAN_POINT('Ctrl Pts',(23.,42.2916666803226,39.8371685740842));
#8409=CARTESIAN_POINT('Ctrl Pts',(12.3256628518317,42.0833333469893,46.));
#8410=CARTESIAN_POINT('Ctrl Pts',(8.45006291411674E-15,41.8750000136559,
46.));
#8411=CARTESIAN_POINT('Ctrl Pts',(-12.3256628518316,41.6666666803226,46.));
#8412=CARTESIAN_POINT('Ctrl Pts',(-23.,41.4583333469893,39.8371685740842));
#8413=CARTESIAN_POINT('Ctrl Pts',(-33.6743371481683,41.2500000136559,33.6743371481684));
#8414=CARTESIAN_POINT('Ctrl Pts',(-39.8371685740842,41.0416666803226,23.));
#8415=CARTESIAN_POINT('Ctrl Pts',(-46.,40.8333333469893,12.3256628518317));
#8416=CARTESIAN_POINT('Ctrl Pts',(-46.,40.6250000136559,0.));
#8417=CARTESIAN_POINT('Ctrl Pts',(-46.,40.4166666803226,-12.3256628518316));
#8418=CARTESIAN_POINT('Ctrl Pts',(-39.8371685740842,40.2083333469893,-23.));
#8419=CARTESIAN_POINT('Ctrl Pts',(-33.6743371481684,40.0000000136559,-33.6743371481684));
#8420=CARTESIAN_POINT('Ctrl Pts',(-23.,39.7916666803226,-39.8371685740842));
#8421=CARTESIAN_POINT('Ctrl Pts',(-12.3256628518317,39.5833333469893,-46.));
#8422=CARTESIAN_POINT('Ctrl Pts',(-2.81668763803891E-15,39.3750000136559,
-46.));
#8423=CARTESIAN_POINT('Ctrl Pts',(12.3256628518316,39.1666666803226,-46.));
#8424=CARTESIAN_POINT('Ctrl Pts',(23.,38.9583333469893,-39.8371685740842));
#8425=CARTESIAN_POINT('Ctrl Pts',(33.6743371481683,38.7500000136559,-33.6743371481684));
#8426=CARTESIAN_POINT('Ctrl Pts',(39.8371685740842,38.5416666803226,-23.));
#8427=CARTESIAN_POINT('Ctrl Pts',(46.,38.3333333469893,-12.3256628518317));
#8428=CARTESIAN_POINT('Ctrl Pts',(46.,38.1250000136559,-5.63337527607782E-15));
#8429=CARTESIAN_POINT('Ctrl Pts',(46.,37.9166666803226,12.3256628518316));
#8430=CARTESIAN_POINT('Ctrl Pts',(39.8371685740842,37.7083333469893,23.));
#8431=CARTESIAN_POINT('Ctrl Pts',(33.6743371481684,37.5000000136559,33.6743371481683));
#8432=CARTESIAN_POINT('Ctrl Pts',(23.,37.2916666803226,39.8371685740842));
#8433=CARTESIAN_POINT('Ctrl Pts',(12.3256628518317,37.0833333469893,46.));
#8434=CARTESIAN_POINT('Ctrl Pts',(8.45006291411674E-15,36.8750000136559,
46.));
#8435=CARTESIAN_POINT('Ctrl Pts',(-12.3256628518316,36.6666666803226,46.));
#8436=CARTESIAN_POINT('Ctrl Pts',(-23.,36.4583333469893,39.8371685740842));
#8437=CARTESIAN_POINT('Ctrl Pts',(-33.6743371481683,36.2500000136559,33.6743371481684));
#8438=CARTESIAN_POINT('Ctrl Pts',(-39.8371685740842,36.0416666803226,23.));
#8439=CARTESIAN_POINT('Ctrl Pts',(-46.,35.8333333469893,12.3256628518317));
#8440=CARTESIAN_POINT('Ctrl Pts',(-46.,35.6250000136559,0.));
#8441=CARTESIAN_POINT('Ctrl Pts',(-46.,35.4166666803226,-12.3256628518316));
#8442=CARTESIAN_POINT('Ctrl Pts',(-39.8371685740842,35.2083333469893,-23.));
#8443=CARTESIAN_POINT('Ctrl Pts',(-33.6743371481684,35.0000000136559,-33.6743371481684));
#8444=CARTESIAN_POINT('Ctrl Pts',(-23.,34.7916666803226,-39.8371685740842));
#8445=CARTESIAN_POINT('Ctrl Pts',(-12.3256628518317,34.5833333469893,-46.));
#8446=CARTESIAN_POINT('Ctrl Pts',(-2.81668763803891E-15,34.3750000136559,
-46.));
#8447=CARTESIAN_POINT('Ctrl Pts',(12.3256628518316,34.1666666803226,-46.));
#8448=CARTESIAN_POINT('Ctrl Pts',(23.,33.9583333469893,-39.8371685740842));
#8449=CARTESIAN_POINT('Ctrl Pts',(33.6743371481683,33.7500000136559,-33.6743371481684));
#8450=CARTESIAN_POINT('Ctrl Pts',(39.8371685740842,33.5416666803226,-23.));
#8451=CARTESIAN_POINT('Ctrl Pts',(46.,33.3333333469893,-12.3256628518317));
#8452=CARTESIAN_POINT('Ctrl Pts',(46.,33.1250000136559,-5.63337527607782E-15));
#8453=CARTESIAN_POINT('Ctrl Pts',(46.,32.9166666803226,12.3256628518316));
#8454=CARTESIAN_POINT('Ctrl Pts',(39.8371685740842,32.7083333469893,23.));
#8455=CARTESIAN_POINT('Ctrl Pts',(33.6743371481684,32.5000000136559,33.6743371481683));
#8456=CARTESIAN_POINT('Ctrl Pts',(23.,32.2916666803226,39.8371685740842));
#8457=CARTESIAN_POINT('Ctrl Pts',(12.3256628518317,32.0833333469893,46.));
#8458=CARTESIAN_POINT('Ctrl Pts',(8.45006291411674E-15,31.8750000136559,
46.));
#8459=CARTESIAN_POINT('Ctrl Pts',(-12.3256628518316,31.6666666803226,46.));
#8460=CARTESIAN_POINT('Ctrl Pts',(-23.,31.4583333469893,39.8371685740842));
#8461=CARTESIAN_POINT('Ctrl Pts',(-33.6743371481683,31.2500000136559,33.6743371481684));
#8462=CARTESIAN_POINT('Ctrl Pts',(-39.8371685740842,31.0416666803226,23.));
#8463=CARTESIAN_POINT('Ctrl Pts',(-46.,30.8333333469893,12.3256628518317));
#8464=CARTESIAN_POINT('Ctrl Pts',(-46.,30.6250000136559,0.));
#8465=CARTESIAN_POINT('Ctrl Pts',(-46.,30.4166666803226,-12.3256628518316));
#8466=CARTESIAN_POINT('Ctrl Pts',(-39.8371685740842,30.2083333469893,-23.));
#8467=CARTESIAN_POINT('Ctrl Pts',(-33.6743371481684,30.0000000136559,-33.6743371481684));
#8468=CARTESIAN_POINT('Ctrl Pts',(-23.,29.7916666803226,-39.8371685740842));
#8469=CARTESIAN_POINT('Ctrl Pts',(-12.3256628518317,29.5833333469893,-46.));
#8470=CARTESIAN_POINT('Ctrl Pts',(-2.81668763803891E-15,29.3750000136559,
-46.));
#8471=CARTESIAN_POINT('Ctrl Pts',(12.3256628518316,29.1666666803226,-46.));
#8472=CARTESIAN_POINT('Ctrl Pts',(23.,28.9583333469893,-39.8371685740842));
#8473=CARTESIAN_POINT('Ctrl Pts',(33.6743371481683,28.7500000136559,-33.6743371481684));
#8474=CARTESIAN_POINT('Ctrl Pts',(39.8371685740842,28.5416666803226,-23.));
#8475=CARTESIAN_POINT('Ctrl Pts',(46.,28.3333333469893,-12.3256628518317));
#8476=CARTESIAN_POINT('Ctrl Pts',(46.,28.1250000136559,-5.63337527607782E-15));
#8477=CARTESIAN_POINT('Ctrl Pts',(46.,27.9166666803226,12.3256628518316));
#8478=CARTESIAN_POINT('Ctrl Pts',(39.8371685740842,27.7083333469893,23.));
#8479=CARTESIAN_POINT('Ctrl Pts',(33.6743371481684,27.5000000136559,33.6743371481683));
#8480=CARTESIAN_POINT('Ctrl Pts',(23.,27.2916666803226,39.8371685740842));
#8481=CARTESIAN_POINT('Ctrl Pts',(12.3256628518317,27.0833333469893,46.));
#8482=CARTESIAN_POINT('Ctrl Pts',(8.45006291411674E-15,26.8750000136559,
46.));
#8483=CARTESIAN_POINT('Ctrl Pts',(-12.3256628518316,26.6666666803226,46.));
#8484=CARTESIAN_POINT('Ctrl Pts',(-23.,26.4583333469893,39.8371685740842));
#8485=CARTESIAN_POINT('Ctrl Pts',(-33.6743371481683,26.2500000136559,33.6743371481684));
#8486=CARTESIAN_POINT('Ctrl Pts',(-39.8371685740842,26.0416666803226,23.));
#8487=CARTESIAN_POINT('Ctrl Pts',(-46.,25.8333333469893,12.3256628518317));
#8488=CARTESIAN_POINT('Ctrl Pts',(-46.,25.6250000136559,0.));
#8489=CARTESIAN_POINT('Ctrl Pts',(-48.706329375,57.187500006828,-1.8898197019151E-14));
#8490=CARTESIAN_POINT('Ctrl Pts',(-48.706329375,56.9791666734946,-13.0508216223155));
#8491=CARTESIAN_POINT('Ctrl Pts',(-42.1809185638422,56.7708333401613,-24.3531646875));
#8492=CARTESIAN_POINT('Ctrl Pts',(-35.6555077526845,56.562500006828,-35.6555077526845));
#8493=CARTESIAN_POINT('Ctrl Pts',(-24.3531646875,56.3541666734946,-42.1809185638423));
#8494=CARTESIAN_POINT('Ctrl Pts',(-13.0508216223155,56.1458333401613,-48.706329375));
#8495=CARTESIAN_POINT('Ctrl Pts',(1.59157945007855E-14,55.937500006828,
-48.706329375));
#8496=CARTESIAN_POINT('Ctrl Pts',(13.0508216223155,55.7291666734946,-48.706329375));
#8497=CARTESIAN_POINT('Ctrl Pts',(24.3531646875,55.5208333401613,-42.1809185638422));
#8498=CARTESIAN_POINT('Ctrl Pts',(35.6555077526845,55.312500006828,-35.6555077526845));
#8499=CARTESIAN_POINT('Ctrl Pts',(42.1809185638422,55.1041666734946,-24.3531646875));
#8500=CARTESIAN_POINT('Ctrl Pts',(48.706329375,54.8958333401613,-13.0508216223155));
#8501=CARTESIAN_POINT('Ctrl Pts',(48.706329375,54.687500006828,1.293339198242E-14));
#8502=CARTESIAN_POINT('Ctrl Pts',(48.706329375,54.4791666734946,13.0508216223155));
#8503=CARTESIAN_POINT('Ctrl Pts',(42.1809185638422,54.2708333401613,24.3531646875));
#8504=CARTESIAN_POINT('Ctrl Pts',(35.6555077526845,54.062500006828,35.6555077526845));
#8505=CARTESIAN_POINT('Ctrl Pts',(24.3531646875,53.8541666734946,42.1809185638422));
#8506=CARTESIAN_POINT('Ctrl Pts',(13.0508216223155,53.6458333401613,48.706329375));
#8507=CARTESIAN_POINT('Ctrl Pts',(-9.95098946405443E-15,53.437500006828,
48.706329375));
#8508=CARTESIAN_POINT('Ctrl Pts',(-13.0508216223155,53.2291666734946,48.706329375));
#8509=CARTESIAN_POINT('Ctrl Pts',(-24.3531646875,53.0208333401613,42.1809185638423));
#8510=CARTESIAN_POINT('Ctrl Pts',(-35.6555077526845,52.812500006828,35.6555077526845));
#8511=CARTESIAN_POINT('Ctrl Pts',(-42.1809185638422,52.6041666734946,24.3531646875));
#8512=CARTESIAN_POINT('Ctrl Pts',(-48.706329375,52.3958333401613,13.0508216223155));
#8513=CARTESIAN_POINT('Ctrl Pts',(-48.706329375,52.187500006828,-1.8898197019151E-14));
#8514=CARTESIAN_POINT('Ctrl Pts',(-48.706329375,51.9791666734946,-13.0508216223155));
#8515=CARTESIAN_POINT('Ctrl Pts',(-42.1809185638422,51.7708333401613,-24.3531646875));
#8516=CARTESIAN_POINT('Ctrl Pts',(-35.6555077526845,51.562500006828,-35.6555077526845));
#8517=CARTESIAN_POINT('Ctrl Pts',(-24.3531646875,51.3541666734946,-42.1809185638423));
#8518=CARTESIAN_POINT('Ctrl Pts',(-13.0508216223155,51.1458333401613,-48.706329375));
#8519=CARTESIAN_POINT('Ctrl Pts',(1.59157945007855E-14,50.937500006828,
-48.706329375));
#8520=CARTESIAN_POINT('Ctrl Pts',(13.0508216223155,50.7291666734946,-48.706329375));
#8521=CARTESIAN_POINT('Ctrl Pts',(24.3531646875,50.5208333401613,-42.1809185638422));
#8522=CARTESIAN_POINT('Ctrl Pts',(35.6555077526845,50.312500006828,-35.6555077526845));
#8523=CARTESIAN_POINT('Ctrl Pts',(42.1809185638422,50.1041666734946,-24.3531646875));
#8524=CARTESIAN_POINT('Ctrl Pts',(48.706329375,49.8958333401613,-13.0508216223155));
#8525=CARTESIAN_POINT('Ctrl Pts',(48.706329375,49.687500006828,1.293339198242E-14));
#8526=CARTESIAN_POINT('Ctrl Pts',(48.706329375,49.4791666734946,13.0508216223155));
#8527=CARTESIAN_POINT('Ctrl Pts',(42.1809185638422,49.2708333401613,24.3531646875));
#8528=CARTESIAN_POINT('Ctrl Pts',(35.6555077526845,49.062500006828,35.6555077526845));
#8529=CARTESIAN_POINT('Ctrl Pts',(24.3531646875,48.8541666734946,42.1809185638422));
#8530=CARTESIAN_POINT('Ctrl Pts',(13.0508216223155,48.6458333401613,48.706329375));
#8531=CARTESIAN_POINT('Ctrl Pts',(-9.95098946405443E-15,48.437500006828,
48.706329375));
#8532=CARTESIAN_POINT('Ctrl Pts',(-13.0508216223155,48.2291666734946,48.706329375));
#8533=CARTESIAN_POINT('Ctrl Pts',(-24.3531646875,48.0208333401613,42.1809185638423));
#8534=CARTESIAN_POINT('Ctrl Pts',(-35.6555077526845,47.812500006828,35.6555077526845));
#8535=CARTESIAN_POINT('Ctrl Pts',(-42.1809185638422,47.6041666734946,24.3531646875));
#8536=CARTESIAN_POINT('Ctrl Pts',(-48.706329375,47.3958333401613,13.0508216223155));
#8537=CARTESIAN_POINT('Ctrl Pts',(-48.706329375,47.187500006828,-1.8898197019151E-14));
#8538=CARTESIAN_POINT('Ctrl Pts',(-48.706329375,46.9791666734946,-13.0508216223155));
#8539=CARTESIAN_POINT('Ctrl Pts',(-42.1809185638422,46.7708333401613,-24.3531646875));
#8540=CARTESIAN_POINT('Ctrl Pts',(-35.6555077526845,46.562500006828,-35.6555077526845));
#8541=CARTESIAN_POINT('Ctrl Pts',(-24.3531646875,46.3541666734946,-42.1809185638423));
#8542=CARTESIAN_POINT('Ctrl Pts',(-13.0508216223155,46.1458333401613,-48.706329375));
#8543=CARTESIAN_POINT('Ctrl Pts',(1.59157945007855E-14,45.937500006828,
-48.706329375));
#8544=CARTESIAN_POINT('Ctrl Pts',(13.0508216223155,45.7291666734946,-48.706329375));
#8545=CARTESIAN_POINT('Ctrl Pts',(24.3531646875,45.5208333401613,-42.1809185638422));
#8546=CARTESIAN_POINT('Ctrl Pts',(35.6555077526845,45.312500006828,-35.6555077526845));
#8547=CARTESIAN_POINT('Ctrl Pts',(42.1809185638422,45.1041666734946,-24.3531646875));
#8548=CARTESIAN_POINT('Ctrl Pts',(48.706329375,44.8958333401613,-13.0508216223155));
#8549=CARTESIAN_POINT('Ctrl Pts',(48.706329375,44.687500006828,1.293339198242E-14));
#8550=CARTESIAN_POINT('Ctrl Pts',(48.706329375,44.4791666734946,13.0508216223155));
#8551=CARTESIAN_POINT('Ctrl Pts',(42.1809185638422,44.2708333401613,24.3531646875));
#8552=CARTESIAN_POINT('Ctrl Pts',(35.6555077526845,44.062500006828,35.6555077526845));
#8553=CARTESIAN_POINT('Ctrl Pts',(24.3531646875,43.8541666734946,42.1809185638422));
#8554=CARTESIAN_POINT('Ctrl Pts',(13.0508216223155,43.6458333401613,48.706329375));
#8555=CARTESIAN_POINT('Ctrl Pts',(-9.95098946405443E-15,43.437500006828,
48.706329375));
#8556=CARTESIAN_POINT('Ctrl Pts',(-13.0508216223155,43.2291666734946,48.706329375));
#8557=CARTESIAN_POINT('Ctrl Pts',(-24.3531646875,43.0208333401613,42.1809185638423));
#8558=CARTESIAN_POINT('Ctrl Pts',(-35.6555077526845,42.812500006828,35.6555077526845));
#8559=CARTESIAN_POINT('Ctrl Pts',(-42.1809185638422,42.6041666734946,24.3531646875));
#8560=CARTESIAN_POINT('Ctrl Pts',(-48.706329375,42.3958333401613,13.0508216223155));
#8561=CARTESIAN_POINT('Ctrl Pts',(-48.706329375,42.187500006828,-1.8898197019151E-14));
#8562=CARTESIAN_POINT('Ctrl Pts',(-48.706329375,41.9791666734946,-13.0508216223155));
#8563=CARTESIAN_POINT('Ctrl Pts',(-42.1809185638422,41.7708333401613,-24.3531646875));
#8564=CARTESIAN_POINT('Ctrl Pts',(-35.6555077526845,41.562500006828,-35.6555077526845));
#8565=CARTESIAN_POINT('Ctrl Pts',(-24.3531646875,41.3541666734946,-42.1809185638423));
#8566=CARTESIAN_POINT('Ctrl Pts',(-13.0508216223155,41.1458333401613,-48.706329375));
#8567=CARTESIAN_POINT('Ctrl Pts',(1.59157945007855E-14,40.937500006828,
-48.706329375));
#8568=CARTESIAN_POINT('Ctrl Pts',(13.0508216223155,40.7291666734946,-48.706329375));
#8569=CARTESIAN_POINT('Ctrl Pts',(24.3531646875,40.5208333401613,-42.1809185638422));
#8570=CARTESIAN_POINT('Ctrl Pts',(35.6555077526845,40.312500006828,-35.6555077526845));
#8571=CARTESIAN_POINT('Ctrl Pts',(42.1809185638422,40.1041666734946,-24.3531646875));
#8572=CARTESIAN_POINT('Ctrl Pts',(48.706329375,39.8958333401613,-13.0508216223155));
#8573=CARTESIAN_POINT('Ctrl Pts',(48.706329375,39.687500006828,1.293339198242E-14));
#8574=CARTESIAN_POINT('Ctrl Pts',(48.706329375,39.4791666734946,13.0508216223155));
#8575=CARTESIAN_POINT('Ctrl Pts',(42.1809185638422,39.2708333401613,24.3531646875));
#8576=CARTESIAN_POINT('Ctrl Pts',(35.6555077526845,39.062500006828,35.6555077526845));
#8577=CARTESIAN_POINT('Ctrl Pts',(24.3531646875,38.8541666734946,42.1809185638422));
#8578=CARTESIAN_POINT('Ctrl Pts',(13.0508216223155,38.6458333401613,48.706329375));
#8579=CARTESIAN_POINT('Ctrl Pts',(-9.95098946405443E-15,38.437500006828,
48.706329375));
#8580=CARTESIAN_POINT('Ctrl Pts',(-13.0508216223155,38.2291666734946,48.706329375));
#8581=CARTESIAN_POINT('Ctrl Pts',(-24.3531646875,38.0208333401613,42.1809185638423));
#8582=CARTESIAN_POINT('Ctrl Pts',(-35.6555077526845,37.812500006828,35.6555077526845));
#8583=CARTESIAN_POINT('Ctrl Pts',(-42.1809185638422,37.6041666734946,24.3531646875));
#8584=CARTESIAN_POINT('Ctrl Pts',(-48.706329375,37.3958333401613,13.0508216223155));
#8585=CARTESIAN_POINT('Ctrl Pts',(-48.706329375,37.187500006828,-1.8898197019151E-14));
#8586=CARTESIAN_POINT('Ctrl Pts',(-48.706329375,36.9791666734946,-13.0508216223155));
#8587=CARTESIAN_POINT('Ctrl Pts',(-42.1809185638422,36.7708333401613,-24.3531646875));
#8588=CARTESIAN_POINT('Ctrl Pts',(-35.6555077526845,36.562500006828,-35.6555077526845));
#8589=CARTESIAN_POINT('Ctrl Pts',(-24.3531646875,36.3541666734946,-42.1809185638423));
#8590=CARTESIAN_POINT('Ctrl Pts',(-13.0508216223155,36.1458333401613,-48.706329375));
#8591=CARTESIAN_POINT('Ctrl Pts',(1.59157945007855E-14,35.937500006828,
-48.706329375));
#8592=CARTESIAN_POINT('Ctrl Pts',(13.0508216223155,35.7291666734946,-48.706329375));
#8593=CARTESIAN_POINT('Ctrl Pts',(24.3531646875,35.5208333401613,-42.1809185638422));
#8594=CARTESIAN_POINT('Ctrl Pts',(35.6555077526845,35.312500006828,-35.6555077526845));
#8595=CARTESIAN_POINT('Ctrl Pts',(42.1809185638422,35.1041666734946,-24.3531646875));
#8596=CARTESIAN_POINT('Ctrl Pts',(48.706329375,34.8958333401613,-13.0508216223155));
#8597=CARTESIAN_POINT('Ctrl Pts',(48.706329375,34.687500006828,1.293339198242E-14));
#8598=CARTESIAN_POINT('Ctrl Pts',(48.706329375,34.4791666734946,13.0508216223155));
#8599=CARTESIAN_POINT('Ctrl Pts',(42.1809185638422,34.2708333401613,24.3531646875));
#8600=CARTESIAN_POINT('Ctrl Pts',(35.6555077526845,34.062500006828,35.6555077526845));
#8601=CARTESIAN_POINT('Ctrl Pts',(24.3531646875,33.8541666734946,42.1809185638422));
#8602=CARTESIAN_POINT('Ctrl Pts',(13.0508216223155,33.6458333401613,48.706329375));
#8603=CARTESIAN_POINT('Ctrl Pts',(-9.95098946405443E-15,33.437500006828,
48.706329375));
#8604=CARTESIAN_POINT('Ctrl Pts',(-13.0508216223155,33.2291666734946,48.706329375));
#8605=CARTESIAN_POINT('Ctrl Pts',(-24.3531646875,33.0208333401613,42.1809185638423));
#8606=CARTESIAN_POINT('Ctrl Pts',(-35.6555077526845,32.812500006828,35.6555077526845));
#8607=CARTESIAN_POINT('Ctrl Pts',(-42.1809185638422,32.6041666734946,24.3531646875));
#8608=CARTESIAN_POINT('Ctrl Pts',(-48.706329375,32.3958333401613,13.0508216223155));
#8609=CARTESIAN_POINT('Ctrl Pts',(-48.706329375,32.187500006828,-1.8898197019151E-14));
#8610=CARTESIAN_POINT('Ctrl Pts',(-48.706329375,31.9791666734946,-13.0508216223155));
#8611=CARTESIAN_POINT('Ctrl Pts',(-42.1809185638422,31.7708333401613,-24.3531646875));
#8612=CARTESIAN_POINT('Ctrl Pts',(-35.6555077526845,31.562500006828,-35.6555077526845));
#8613=CARTESIAN_POINT('Ctrl Pts',(-24.3531646875,31.3541666734946,-42.1809185638423));
#8614=CARTESIAN_POINT('Ctrl Pts',(-13.0508216223155,31.1458333401613,-48.706329375));
#8615=CARTESIAN_POINT('Ctrl Pts',(1.59157945007855E-14,30.937500006828,
-48.706329375));
#8616=CARTESIAN_POINT('Ctrl Pts',(13.0508216223155,30.7291666734946,-48.706329375));
#8617=CARTESIAN_POINT('Ctrl Pts',(24.3531646875,30.5208333401613,-42.1809185638422));
#8618=CARTESIAN_POINT('Ctrl Pts',(35.6555077526845,30.312500006828,-35.6555077526845));
#8619=CARTESIAN_POINT('Ctrl Pts',(42.1809185638422,30.1041666734946,-24.3531646875));
#8620=CARTESIAN_POINT('Ctrl Pts',(48.706329375,29.8958333401613,-13.0508216223155));
#8621=CARTESIAN_POINT('Ctrl Pts',(48.706329375,29.687500006828,1.293339198242E-14));
#8622=CARTESIAN_POINT('Ctrl Pts',(48.706329375,29.4791666734946,13.0508216223155));
#8623=CARTESIAN_POINT('Ctrl Pts',(42.1809185638422,29.2708333401613,24.3531646875));
#8624=CARTESIAN_POINT('Ctrl Pts',(35.6555077526845,29.062500006828,35.6555077526845));
#8625=CARTESIAN_POINT('Ctrl Pts',(24.3531646875,28.8541666734946,42.1809185638422));
#8626=CARTESIAN_POINT('Ctrl Pts',(13.0508216223155,28.6458333401613,48.706329375));
#8627=CARTESIAN_POINT('Ctrl Pts',(-9.95098946405443E-15,28.437500006828,
48.706329375));
#8628=CARTESIAN_POINT('Ctrl Pts',(-13.0508216223155,28.2291666734946,48.706329375));
#8629=CARTESIAN_POINT('Ctrl Pts',(-24.3531646875,28.0208333401613,42.1809185638423));
#8630=CARTESIAN_POINT('Ctrl Pts',(-35.6555077526845,27.812500006828,35.6555077526845));
#8631=CARTESIAN_POINT('Ctrl Pts',(-42.1809185638422,27.6041666734946,24.3531646875));
#8632=CARTESIAN_POINT('Ctrl Pts',(-48.706329375,27.3958333401613,13.0508216223155));
#8633=CARTESIAN_POINT('Ctrl Pts',(-48.706329375,27.187500006828,-1.8898197019151E-14));
#8634=CARTESIAN_POINT('',(-48.5134353784345,52.1175463684955,-4.33048599679673));
#8635=CARTESIAN_POINT('Ctrl Pts',(-45.7957082162897,50.5508791552084,-4.33048599679673));
#8636=CARTESIAN_POINT('Ctrl Pts',(-46.027322302781,50.6843839384496,-4.33048599679671));
#8637=CARTESIAN_POINT('Ctrl Pts',(-46.4905476657728,50.9513983799648,-4.33048599679678));
#8638=CARTESIAN_POINT('Ctrl Pts',(-46.9537676533565,51.2184221466352,-4.33048599679674));
#8639=CARTESIAN_POINT('Ctrl Pts',(-47.6280672732222,51.6071316973962,-4.33048599679674));
#8640=CARTESIAN_POINT('Ctrl Pts',(-48.0707534890442,51.8623352807796,-4.33048599679674));
#8641=CARTESIAN_POINT('Ctrl Pts',(-48.5134353784345,52.1175463684955,-4.33048599679673));
#8642=CARTESIAN_POINT('',(-4.32456003949876,51.0073567866782,-48.5139639861634));
#8643=CARTESIAN_POINT('Ctrl Pts',(-48.5134353784345,52.1175463684955,-4.33048599679674));
#8644=CARTESIAN_POINT('Ctrl Pts',(-47.5573898704235,51.9424850907232,-15.0408432190651));
#8645=CARTESIAN_POINT('Ctrl Pts',(-42.1809185638422,51.7708333401613,-24.3531646875));
#8646=CARTESIAN_POINT('Ctrl Pts',(-35.6555077526845,51.562500006828,-35.6555077526845));
#8647=CARTESIAN_POINT('Ctrl Pts',(-24.3531646875,51.3541666734946,-42.1809185638423));
#8648=CARTESIAN_POINT('Ctrl Pts',(-15.038141415499,51.1824651212465,-47.5589497574396));
#8649=CARTESIAN_POINT('Ctrl Pts',(-4.32456003949876,51.0073567866782,-48.5139639861634));
#8650=CARTESIAN_POINT('Origin',(-4.32455765124451,8022.20454033029,4524.01087378963));
#8651=CARTESIAN_POINT('Ctrl Pts',(-46.,55.6250000136559,0.));
#8652=CARTESIAN_POINT('Ctrl Pts',(-46.,55.4166666803226,-12.3256628518316));
#8653=CARTESIAN_POINT('Ctrl Pts',(-39.8371685740842,55.2083333469893,-23.));
#8654=CARTESIAN_POINT('Ctrl Pts',(-33.6743371481684,55.0000000136559,-33.6743371481684));
#8655=CARTESIAN_POINT('Ctrl Pts',(-23.,54.7916666803226,-39.8371685740842));
#8656=CARTESIAN_POINT('Ctrl Pts',(-12.3256628518317,54.5833333469893,-46.));
#8657=CARTESIAN_POINT('Ctrl Pts',(-2.81668763803891E-15,54.3750000136559,
-46.));
#8658=CARTESIAN_POINT('Ctrl Pts',(12.3256628518316,54.1666666803226,-46.));
#8659=CARTESIAN_POINT('Ctrl Pts',(23.,53.9583333469893,-39.8371685740842));
#8660=CARTESIAN_POINT('Ctrl Pts',(33.6743371481683,53.7500000136559,-33.6743371481684));
#8661=CARTESIAN_POINT('Ctrl Pts',(39.8371685740842,53.5416666803226,-23.));
#8662=CARTESIAN_POINT('Ctrl Pts',(46.,53.3333333469893,-12.3256628518317));
#8663=CARTESIAN_POINT('Ctrl Pts',(46.,53.1250000136559,-5.63337527607782E-15));
#8664=CARTESIAN_POINT('Ctrl Pts',(46.,52.9166666803226,12.3256628518316));
#8665=CARTESIAN_POINT('Ctrl Pts',(39.8371685740842,52.7083333469893,23.));
#8666=CARTESIAN_POINT('Ctrl Pts',(33.6743371481684,52.5000000136559,33.6743371481683));
#8667=CARTESIAN_POINT('Ctrl Pts',(23.,52.2916666803226,39.8371685740842));
#8668=CARTESIAN_POINT('Ctrl Pts',(12.3256628518317,52.0833333469893,46.));
#8669=CARTESIAN_POINT('Ctrl Pts',(8.45006291411674E-15,51.8750000136559,
46.));
#8670=CARTESIAN_POINT('Ctrl Pts',(-12.3256628518316,51.6666666803226,46.));
#8671=CARTESIAN_POINT('Ctrl Pts',(-23.,51.4583333469893,39.8371685740842));
#8672=CARTESIAN_POINT('Ctrl Pts',(-33.6743371481683,51.2500000136559,33.6743371481684));
#8673=CARTESIAN_POINT('Ctrl Pts',(-39.8371685740842,51.0416666803226,23.));
#8674=CARTESIAN_POINT('Ctrl Pts',(-46.,50.8333333469893,12.3256628518317));
#8675=CARTESIAN_POINT('Ctrl Pts',(-46.,50.6250000136559,0.));
#8676=CARTESIAN_POINT('Ctrl Pts',(-46.,50.4166666803226,-12.3256628518316));
#8677=CARTESIAN_POINT('Ctrl Pts',(-39.8371685740842,50.2083333469893,-23.));
#8678=CARTESIAN_POINT('Ctrl Pts',(-33.6743371481684,50.0000000136559,-33.6743371481684));
#8679=CARTESIAN_POINT('Ctrl Pts',(-23.,49.7916666803226,-39.8371685740842));
#8680=CARTESIAN_POINT('Ctrl Pts',(-12.3256628518317,49.5833333469893,-46.));
#8681=CARTESIAN_POINT('Ctrl Pts',(-2.81668763803891E-15,49.3750000136559,
-46.));
#8682=CARTESIAN_POINT('Ctrl Pts',(12.3256628518316,49.1666666803226,-46.));
#8683=CARTESIAN_POINT('Ctrl Pts',(23.,48.9583333469893,-39.8371685740842));
#8684=CARTESIAN_POINT('Ctrl Pts',(33.6743371481683,48.7500000136559,-33.6743371481684));
#8685=CARTESIAN_POINT('Ctrl Pts',(39.8371685740842,48.5416666803226,-23.));
#8686=CARTESIAN_POINT('Ctrl Pts',(46.,48.3333333469893,-12.3256628518317));
#8687=CARTESIAN_POINT('Ctrl Pts',(46.,48.1250000136559,-5.63337527607782E-15));
#8688=CARTESIAN_POINT('Ctrl Pts',(46.,47.9166666803226,12.3256628518316));
#8689=CARTESIAN_POINT('Ctrl Pts',(39.8371685740842,47.7083333469893,23.));
#8690=CARTESIAN_POINT('Ctrl Pts',(33.6743371481684,47.5000000136559,33.6743371481683));
#8691=CARTESIAN_POINT('Ctrl Pts',(23.,47.2916666803226,39.8371685740842));
#8692=CARTESIAN_POINT('Ctrl Pts',(12.3256628518317,47.0833333469893,46.));
#8693=CARTESIAN_POINT('Ctrl Pts',(8.45006291411674E-15,46.8750000136559,
46.));
#8694=CARTESIAN_POINT('Ctrl Pts',(-12.3256628518316,46.6666666803226,46.));
#8695=CARTESIAN_POINT('Ctrl Pts',(-23.,46.4583333469893,39.8371685740842));
#8696=CARTESIAN_POINT('Ctrl Pts',(-33.6743371481683,46.2500000136559,33.6743371481684));
#8697=CARTESIAN_POINT('Ctrl Pts',(-39.8371685740842,46.0416666803226,23.));
#8698=CARTESIAN_POINT('Ctrl Pts',(-46.,45.8333333469892,12.3256628518317));
#8699=CARTESIAN_POINT('Ctrl Pts',(-46.,45.6250000136559,0.));
#8700=CARTESIAN_POINT('Ctrl Pts',(-46.,45.4166666803226,-12.3256628518316));
#8701=CARTESIAN_POINT('Ctrl Pts',(-39.8371685740842,45.2083333469893,-23.));
#8702=CARTESIAN_POINT('Ctrl Pts',(-33.6743371481684,45.0000000136559,-33.6743371481684));
#8703=CARTESIAN_POINT('Ctrl Pts',(-23.,44.7916666803226,-39.8371685740842));
#8704=CARTESIAN_POINT('Ctrl Pts',(-12.3256628518317,44.5833333469893,-46.));
#8705=CARTESIAN_POINT('Ctrl Pts',(-2.81668763803891E-15,44.3750000136559,
-46.));
#8706=CARTESIAN_POINT('Ctrl Pts',(12.3256628518316,44.1666666803226,-46.));
#8707=CARTESIAN_POINT('Ctrl Pts',(23.,43.9583333469893,-39.8371685740842));
#8708=CARTESIAN_POINT('Ctrl Pts',(33.6743371481683,43.7500000136559,-33.6743371481684));
#8709=CARTESIAN_POINT('Ctrl Pts',(39.8371685740842,43.5416666803226,-23.));
#8710=CARTESIAN_POINT('Ctrl Pts',(46.,43.3333333469893,-12.3256628518317));
#8711=CARTESIAN_POINT('Ctrl Pts',(46.,43.1250000136559,-5.63337527607782E-15));
#8712=CARTESIAN_POINT('Ctrl Pts',(46.,42.9166666803226,12.3256628518316));
#8713=CARTESIAN_POINT('Ctrl Pts',(39.8371685740842,42.7083333469893,23.));
#8714=CARTESIAN_POINT('Ctrl Pts',(33.6743371481684,42.5000000136559,33.6743371481683));
#8715=CARTESIAN_POINT('Ctrl Pts',(23.,42.2916666803226,39.8371685740842));
#8716=CARTESIAN_POINT('Ctrl Pts',(12.3256628518317,42.0833333469893,46.));
#8717=CARTESIAN_POINT('Ctrl Pts',(8.45006291411674E-15,41.8750000136559,
46.));
#8718=CARTESIAN_POINT('Ctrl Pts',(-12.3256628518316,41.6666666803226,46.));
#8719=CARTESIAN_POINT('Ctrl Pts',(-23.,41.4583333469893,39.8371685740842));
#8720=CARTESIAN_POINT('Ctrl Pts',(-33.6743371481683,41.2500000136559,33.6743371481684));
#8721=CARTESIAN_POINT('Ctrl Pts',(-39.8371685740842,41.0416666803226,23.));
#8722=CARTESIAN_POINT('Ctrl Pts',(-46.,40.8333333469893,12.3256628518317));
#8723=CARTESIAN_POINT('Ctrl Pts',(-46.,40.6250000136559,0.));
#8724=CARTESIAN_POINT('Ctrl Pts',(-46.,40.4166666803226,-12.3256628518316));
#8725=CARTESIAN_POINT('Ctrl Pts',(-39.8371685740842,40.2083333469893,-23.));
#8726=CARTESIAN_POINT('Ctrl Pts',(-33.6743371481684,40.0000000136559,-33.6743371481684));
#8727=CARTESIAN_POINT('Ctrl Pts',(-23.,39.7916666803226,-39.8371685740842));
#8728=CARTESIAN_POINT('Ctrl Pts',(-12.3256628518317,39.5833333469893,-46.));
#8729=CARTESIAN_POINT('Ctrl Pts',(-2.81668763803891E-15,39.3750000136559,
-46.));
#8730=CARTESIAN_POINT('Ctrl Pts',(12.3256628518316,39.1666666803226,-46.));
#8731=CARTESIAN_POINT('Ctrl Pts',(23.,38.9583333469893,-39.8371685740842));
#8732=CARTESIAN_POINT('Ctrl Pts',(33.6743371481683,38.7500000136559,-33.6743371481684));
#8733=CARTESIAN_POINT('Ctrl Pts',(39.8371685740842,38.5416666803226,-23.));
#8734=CARTESIAN_POINT('Ctrl Pts',(46.,38.3333333469893,-12.3256628518317));
#8735=CARTESIAN_POINT('Ctrl Pts',(46.,38.1250000136559,-5.63337527607782E-15));
#8736=CARTESIAN_POINT('Ctrl Pts',(46.,37.9166666803226,12.3256628518316));
#8737=CARTESIAN_POINT('Ctrl Pts',(39.8371685740842,37.7083333469893,23.));
#8738=CARTESIAN_POINT('Ctrl Pts',(33.6743371481684,37.5000000136559,33.6743371481683));
#8739=CARTESIAN_POINT('Ctrl Pts',(23.,37.2916666803226,39.8371685740842));
#8740=CARTESIAN_POINT('Ctrl Pts',(12.3256628518317,37.0833333469893,46.));
#8741=CARTESIAN_POINT('Ctrl Pts',(8.45006291411674E-15,36.8750000136559,
46.));
#8742=CARTESIAN_POINT('Ctrl Pts',(-12.3256628518316,36.6666666803226,46.));
#8743=CARTESIAN_POINT('Ctrl Pts',(-23.,36.4583333469893,39.8371685740842));
#8744=CARTESIAN_POINT('Ctrl Pts',(-33.6743371481683,36.2500000136559,33.6743371481684));
#8745=CARTESIAN_POINT('Ctrl Pts',(-39.8371685740842,36.0416666803226,23.));
#8746=CARTESIAN_POINT('Ctrl Pts',(-46.,35.8333333469893,12.3256628518317));
#8747=CARTESIAN_POINT('Ctrl Pts',(-46.,35.6250000136559,0.));
#8748=CARTESIAN_POINT('Ctrl Pts',(-46.,35.4166666803226,-12.3256628518316));
#8749=CARTESIAN_POINT('Ctrl Pts',(-39.8371685740842,35.2083333469893,-23.));
#8750=CARTESIAN_POINT('Ctrl Pts',(-33.6743371481684,35.0000000136559,-33.6743371481684));
#8751=CARTESIAN_POINT('Ctrl Pts',(-23.,34.7916666803226,-39.8371685740842));
#8752=CARTESIAN_POINT('Ctrl Pts',(-12.3256628518317,34.5833333469893,-46.));
#8753=CARTESIAN_POINT('Ctrl Pts',(-2.81668763803891E-15,34.3750000136559,
-46.));
#8754=CARTESIAN_POINT('Ctrl Pts',(12.3256628518316,34.1666666803226,-46.));
#8755=CARTESIAN_POINT('Ctrl Pts',(23.,33.9583333469893,-39.8371685740842));
#8756=CARTESIAN_POINT('Ctrl Pts',(33.6743371481683,33.7500000136559,-33.6743371481684));
#8757=CARTESIAN_POINT('Ctrl Pts',(39.8371685740842,33.5416666803226,-23.));
#8758=CARTESIAN_POINT('Ctrl Pts',(46.,33.3333333469893,-12.3256628518317));
#8759=CARTESIAN_POINT('Ctrl Pts',(46.,33.1250000136559,-5.63337527607782E-15));
#8760=CARTESIAN_POINT('Ctrl Pts',(46.,32.9166666803226,12.3256628518316));
#8761=CARTESIAN_POINT('Ctrl Pts',(39.8371685740842,32.7083333469893,23.));
#8762=CARTESIAN_POINT('Ctrl Pts',(33.6743371481684,32.5000000136559,33.6743371481683));
#8763=CARTESIAN_POINT('Ctrl Pts',(23.,32.2916666803226,39.8371685740842));
#8764=CARTESIAN_POINT('Ctrl Pts',(12.3256628518317,32.0833333469893,46.));
#8765=CARTESIAN_POINT('Ctrl Pts',(8.45006291411674E-15,31.8750000136559,
46.));
#8766=CARTESIAN_POINT('Ctrl Pts',(-12.3256628518316,31.6666666803226,46.));
#8767=CARTESIAN_POINT('Ctrl Pts',(-23.,31.4583333469893,39.8371685740842));
#8768=CARTESIAN_POINT('Ctrl Pts',(-33.6743371481683,31.2500000136559,33.6743371481684));
#8769=CARTESIAN_POINT('Ctrl Pts',(-39.8371685740842,31.0416666803226,23.));
#8770=CARTESIAN_POINT('Ctrl Pts',(-46.,30.8333333469893,12.3256628518317));
#8771=CARTESIAN_POINT('Ctrl Pts',(-46.,30.6250000136559,0.));
#8772=CARTESIAN_POINT('Ctrl Pts',(-46.,30.4166666803226,-12.3256628518316));
#8773=CARTESIAN_POINT('Ctrl Pts',(-39.8371685740842,30.2083333469893,-23.));
#8774=CARTESIAN_POINT('Ctrl Pts',(-33.6743371481684,30.0000000136559,-33.6743371481684));
#8775=CARTESIAN_POINT('Ctrl Pts',(-23.,29.7916666803226,-39.8371685740842));
#8776=CARTESIAN_POINT('Ctrl Pts',(-12.3256628518317,29.5833333469893,-46.));
#8777=CARTESIAN_POINT('Ctrl Pts',(-2.81668763803891E-15,29.3750000136559,
-46.));
#8778=CARTESIAN_POINT('Ctrl Pts',(12.3256628518316,29.1666666803226,-46.));
#8779=CARTESIAN_POINT('Ctrl Pts',(23.,28.9583333469893,-39.8371685740842));
#8780=CARTESIAN_POINT('Ctrl Pts',(33.6743371481683,28.7500000136559,-33.6743371481684));
#8781=CARTESIAN_POINT('Ctrl Pts',(39.8371685740842,28.5416666803226,-23.));
#8782=CARTESIAN_POINT('Ctrl Pts',(46.,28.3333333469893,-12.3256628518317));
#8783=CARTESIAN_POINT('Ctrl Pts',(46.,28.1250000136559,-5.63337527607782E-15));
#8784=CARTESIAN_POINT('Ctrl Pts',(46.,27.9166666803226,12.3256628518316));
#8785=CARTESIAN_POINT('Ctrl Pts',(39.8371685740842,27.7083333469893,23.));
#8786=CARTESIAN_POINT('Ctrl Pts',(33.6743371481684,27.5000000136559,33.6743371481683));
#8787=CARTESIAN_POINT('Ctrl Pts',(23.,27.2916666803226,39.8371685740842));
#8788=CARTESIAN_POINT('Ctrl Pts',(12.3256628518317,27.0833333469893,46.));
#8789=CARTESIAN_POINT('Ctrl Pts',(8.45006291411674E-15,26.8750000136559,
46.));
#8790=CARTESIAN_POINT('Ctrl Pts',(-12.3256628518316,26.6666666803226,46.));
#8791=CARTESIAN_POINT('Ctrl Pts',(-23.,26.4583333469893,39.8371685740842));
#8792=CARTESIAN_POINT('Ctrl Pts',(-33.6743371481683,26.2500000136559,33.6743371481684));
#8793=CARTESIAN_POINT('Ctrl Pts',(-39.8371685740842,26.0416666803226,23.));
#8794=CARTESIAN_POINT('Ctrl Pts',(-46.,25.8333333469893,12.3256628518317));
#8795=CARTESIAN_POINT('Ctrl Pts',(-46.,25.6250000136559,0.));
#8796=CARTESIAN_POINT('Ctrl Pts',(-48.706329375,57.187500006828,-1.8898197019151E-14));
#8797=CARTESIAN_POINT('Ctrl Pts',(-48.706329375,56.9791666734946,-13.0508216223155));
#8798=CARTESIAN_POINT('Ctrl Pts',(-42.1809185638422,56.7708333401613,-24.3531646875));
#8799=CARTESIAN_POINT('Ctrl Pts',(-35.6555077526845,56.562500006828,-35.6555077526845));
#8800=CARTESIAN_POINT('Ctrl Pts',(-24.3531646875,56.3541666734946,-42.1809185638423));
#8801=CARTESIAN_POINT('Ctrl Pts',(-13.0508216223155,56.1458333401613,-48.706329375));
#8802=CARTESIAN_POINT('Ctrl Pts',(1.59157945007855E-14,55.937500006828,
-48.706329375));
#8803=CARTESIAN_POINT('Ctrl Pts',(13.0508216223155,55.7291666734946,-48.706329375));
#8804=CARTESIAN_POINT('Ctrl Pts',(24.3531646875,55.5208333401613,-42.1809185638422));
#8805=CARTESIAN_POINT('Ctrl Pts',(35.6555077526845,55.312500006828,-35.6555077526845));
#8806=CARTESIAN_POINT('Ctrl Pts',(42.1809185638422,55.1041666734946,-24.3531646875));
#8807=CARTESIAN_POINT('Ctrl Pts',(48.706329375,54.8958333401613,-13.0508216223155));
#8808=CARTESIAN_POINT('Ctrl Pts',(48.706329375,54.687500006828,1.293339198242E-14));
#8809=CARTESIAN_POINT('Ctrl Pts',(48.706329375,54.4791666734946,13.0508216223155));
#8810=CARTESIAN_POINT('Ctrl Pts',(42.1809185638422,54.2708333401613,24.3531646875));
#8811=CARTESIAN_POINT('Ctrl Pts',(35.6555077526845,54.062500006828,35.6555077526845));
#8812=CARTESIAN_POINT('Ctrl Pts',(24.3531646875,53.8541666734946,42.1809185638422));
#8813=CARTESIAN_POINT('Ctrl Pts',(13.0508216223155,53.6458333401613,48.706329375));
#8814=CARTESIAN_POINT('Ctrl Pts',(-9.95098946405443E-15,53.437500006828,
48.706329375));
#8815=CARTESIAN_POINT('Ctrl Pts',(-13.0508216223155,53.2291666734946,48.706329375));
#8816=CARTESIAN_POINT('Ctrl Pts',(-24.3531646875,53.0208333401613,42.1809185638423));
#8817=CARTESIAN_POINT('Ctrl Pts',(-35.6555077526845,52.812500006828,35.6555077526845));
#8818=CARTESIAN_POINT('Ctrl Pts',(-42.1809185638422,52.6041666734946,24.3531646875));
#8819=CARTESIAN_POINT('Ctrl Pts',(-48.706329375,52.3958333401613,13.0508216223155));
#8820=CARTESIAN_POINT('Ctrl Pts',(-48.706329375,52.187500006828,-1.8898197019151E-14));
#8821=CARTESIAN_POINT('Ctrl Pts',(-48.706329375,51.9791666734946,-13.0508216223155));
#8822=CARTESIAN_POINT('Ctrl Pts',(-42.1809185638422,51.7708333401613,-24.3531646875));
#8823=CARTESIAN_POINT('Ctrl Pts',(-35.6555077526845,51.562500006828,-35.6555077526845));
#8824=CARTESIAN_POINT('Ctrl Pts',(-24.3531646875,51.3541666734946,-42.1809185638423));
#8825=CARTESIAN_POINT('Ctrl Pts',(-13.0508216223155,51.1458333401613,-48.706329375));
#8826=CARTESIAN_POINT('Ctrl Pts',(1.59157945007855E-14,50.937500006828,
-48.706329375));
#8827=CARTESIAN_POINT('Ctrl Pts',(13.0508216223155,50.7291666734946,-48.706329375));
#8828=CARTESIAN_POINT('Ctrl Pts',(24.3531646875,50.5208333401613,-42.1809185638422));
#8829=CARTESIAN_POINT('Ctrl Pts',(35.6555077526845,50.312500006828,-35.6555077526845));
#8830=CARTESIAN_POINT('Ctrl Pts',(42.1809185638422,50.1041666734946,-24.3531646875));
#8831=CARTESIAN_POINT('Ctrl Pts',(48.706329375,49.8958333401613,-13.0508216223155));
#8832=CARTESIAN_POINT('Ctrl Pts',(48.706329375,49.687500006828,1.293339198242E-14));
#8833=CARTESIAN_POINT('Ctrl Pts',(48.706329375,49.4791666734946,13.0508216223155));
#8834=CARTESIAN_POINT('Ctrl Pts',(42.1809185638422,49.2708333401613,24.3531646875));
#8835=CARTESIAN_POINT('Ctrl Pts',(35.6555077526845,49.062500006828,35.6555077526845));
#8836=CARTESIAN_POINT('Ctrl Pts',(24.3531646875,48.8541666734946,42.1809185638422));
#8837=CARTESIAN_POINT('Ctrl Pts',(13.0508216223155,48.6458333401613,48.706329375));
#8838=CARTESIAN_POINT('Ctrl Pts',(-9.95098946405443E-15,48.437500006828,
48.706329375));
#8839=CARTESIAN_POINT('Ctrl Pts',(-13.0508216223155,48.2291666734946,48.706329375));
#8840=CARTESIAN_POINT('Ctrl Pts',(-24.3531646875,48.0208333401613,42.1809185638423));
#8841=CARTESIAN_POINT('Ctrl Pts',(-35.6555077526845,47.812500006828,35.6555077526845));
#8842=CARTESIAN_POINT('Ctrl Pts',(-42.1809185638422,47.6041666734946,24.3531646875));
#8843=CARTESIAN_POINT('Ctrl Pts',(-48.706329375,47.3958333401613,13.0508216223155));
#8844=CARTESIAN_POINT('Ctrl Pts',(-48.706329375,47.187500006828,-1.8898197019151E-14));
#8845=CARTESIAN_POINT('Ctrl Pts',(-48.706329375,46.9791666734946,-13.0508216223155));
#8846=CARTESIAN_POINT('Ctrl Pts',(-42.1809185638422,46.7708333401613,-24.3531646875));
#8847=CARTESIAN_POINT('Ctrl Pts',(-35.6555077526845,46.562500006828,-35.6555077526845));
#8848=CARTESIAN_POINT('Ctrl Pts',(-24.3531646875,46.3541666734946,-42.1809185638423));
#8849=CARTESIAN_POINT('Ctrl Pts',(-13.0508216223155,46.1458333401613,-48.706329375));
#8850=CARTESIAN_POINT('Ctrl Pts',(1.59157945007855E-14,45.937500006828,
-48.706329375));
#8851=CARTESIAN_POINT('Ctrl Pts',(13.0508216223155,45.7291666734946,-48.706329375));
#8852=CARTESIAN_POINT('Ctrl Pts',(24.3531646875,45.5208333401613,-42.1809185638422));
#8853=CARTESIAN_POINT('Ctrl Pts',(35.6555077526845,45.312500006828,-35.6555077526845));
#8854=CARTESIAN_POINT('Ctrl Pts',(42.1809185638422,45.1041666734946,-24.3531646875));
#8855=CARTESIAN_POINT('Ctrl Pts',(48.706329375,44.8958333401613,-13.0508216223155));
#8856=CARTESIAN_POINT('Ctrl Pts',(48.706329375,44.687500006828,1.293339198242E-14));
#8857=CARTESIAN_POINT('Ctrl Pts',(48.706329375,44.4791666734946,13.0508216223155));
#8858=CARTESIAN_POINT('Ctrl Pts',(42.1809185638422,44.2708333401613,24.3531646875));
#8859=CARTESIAN_POINT('Ctrl Pts',(35.6555077526845,44.062500006828,35.6555077526845));
#8860=CARTESIAN_POINT('Ctrl Pts',(24.3531646875,43.8541666734946,42.1809185638422));
#8861=CARTESIAN_POINT('Ctrl Pts',(13.0508216223155,43.6458333401613,48.706329375));
#8862=CARTESIAN_POINT('Ctrl Pts',(-9.95098946405443E-15,43.437500006828,
48.706329375));
#8863=CARTESIAN_POINT('Ctrl Pts',(-13.0508216223155,43.2291666734946,48.706329375));
#8864=CARTESIAN_POINT('Ctrl Pts',(-24.3531646875,43.0208333401613,42.1809185638423));
#8865=CARTESIAN_POINT('Ctrl Pts',(-35.6555077526845,42.812500006828,35.6555077526845));
#8866=CARTESIAN_POINT('Ctrl Pts',(-42.1809185638422,42.6041666734946,24.3531646875));
#8867=CARTESIAN_POINT('Ctrl Pts',(-48.706329375,42.3958333401613,13.0508216223155));
#8868=CARTESIAN_POINT('Ctrl Pts',(-48.706329375,42.187500006828,-1.8898197019151E-14));
#8869=CARTESIAN_POINT('Ctrl Pts',(-48.706329375,41.9791666734946,-13.0508216223155));
#8870=CARTESIAN_POINT('Ctrl Pts',(-42.1809185638422,41.7708333401613,-24.3531646875));
#8871=CARTESIAN_POINT('Ctrl Pts',(-35.6555077526845,41.562500006828,-35.6555077526845));
#8872=CARTESIAN_POINT('Ctrl Pts',(-24.3531646875,41.3541666734946,-42.1809185638423));
#8873=CARTESIAN_POINT('Ctrl Pts',(-13.0508216223155,41.1458333401613,-48.706329375));
#8874=CARTESIAN_POINT('Ctrl Pts',(1.59157945007855E-14,40.937500006828,
-48.706329375));
#8875=CARTESIAN_POINT('Ctrl Pts',(13.0508216223155,40.7291666734946,-48.706329375));
#8876=CARTESIAN_POINT('Ctrl Pts',(24.3531646875,40.5208333401613,-42.1809185638422));
#8877=CARTESIAN_POINT('Ctrl Pts',(35.6555077526845,40.312500006828,-35.6555077526845));
#8878=CARTESIAN_POINT('Ctrl Pts',(42.1809185638422,40.1041666734946,-24.3531646875));
#8879=CARTESIAN_POINT('Ctrl Pts',(48.706329375,39.8958333401613,-13.0508216223155));
#8880=CARTESIAN_POINT('Ctrl Pts',(48.706329375,39.687500006828,1.293339198242E-14));
#8881=CARTESIAN_POINT('Ctrl Pts',(48.706329375,39.4791666734946,13.0508216223155));
#8882=CARTESIAN_POINT('Ctrl Pts',(42.1809185638422,39.2708333401613,24.3531646875));
#8883=CARTESIAN_POINT('Ctrl Pts',(35.6555077526845,39.062500006828,35.6555077526845));
#8884=CARTESIAN_POINT('Ctrl Pts',(24.3531646875,38.8541666734946,42.1809185638422));
#8885=CARTESIAN_POINT('Ctrl Pts',(13.0508216223155,38.6458333401613,48.706329375));
#8886=CARTESIAN_POINT('Ctrl Pts',(-9.95098946405443E-15,38.437500006828,
48.706329375));
#8887=CARTESIAN_POINT('Ctrl Pts',(-13.0508216223155,38.2291666734946,48.706329375));
#8888=CARTESIAN_POINT('Ctrl Pts',(-24.3531646875,38.0208333401613,42.1809185638423));
#8889=CARTESIAN_POINT('Ctrl Pts',(-35.6555077526845,37.812500006828,35.6555077526845));
#8890=CARTESIAN_POINT('Ctrl Pts',(-42.1809185638422,37.6041666734946,24.3531646875));
#8891=CARTESIAN_POINT('Ctrl Pts',(-48.706329375,37.3958333401613,13.0508216223155));
#8892=CARTESIAN_POINT('Ctrl Pts',(-48.706329375,37.187500006828,-1.8898197019151E-14));
#8893=CARTESIAN_POINT('Ctrl Pts',(-48.706329375,36.9791666734946,-13.0508216223155));
#8894=CARTESIAN_POINT('Ctrl Pts',(-42.1809185638422,36.7708333401613,-24.3531646875));
#8895=CARTESIAN_POINT('Ctrl Pts',(-35.6555077526845,36.562500006828,-35.6555077526845));
#8896=CARTESIAN_POINT('Ctrl Pts',(-24.3531646875,36.3541666734946,-42.1809185638423));
#8897=CARTESIAN_POINT('Ctrl Pts',(-13.0508216223155,36.1458333401613,-48.706329375));
#8898=CARTESIAN_POINT('Ctrl Pts',(1.59157945007855E-14,35.937500006828,
-48.706329375));
#8899=CARTESIAN_POINT('Ctrl Pts',(13.0508216223155,35.7291666734946,-48.706329375));
#8900=CARTESIAN_POINT('Ctrl Pts',(24.3531646875,35.5208333401613,-42.1809185638422));
#8901=CARTESIAN_POINT('Ctrl Pts',(35.6555077526845,35.312500006828,-35.6555077526845));
#8902=CARTESIAN_POINT('Ctrl Pts',(42.1809185638422,35.1041666734946,-24.3531646875));
#8903=CARTESIAN_POINT('Ctrl Pts',(48.706329375,34.8958333401613,-13.0508216223155));
#8904=CARTESIAN_POINT('Ctrl Pts',(48.706329375,34.687500006828,1.293339198242E-14));
#8905=CARTESIAN_POINT('Ctrl Pts',(48.706329375,34.4791666734946,13.0508216223155));
#8906=CARTESIAN_POINT('Ctrl Pts',(42.1809185638422,34.2708333401613,24.3531646875));
#8907=CARTESIAN_POINT('Ctrl Pts',(35.6555077526845,34.062500006828,35.6555077526845));
#8908=CARTESIAN_POINT('Ctrl Pts',(24.3531646875,33.8541666734946,42.1809185638422));
#8909=CARTESIAN_POINT('Ctrl Pts',(13.0508216223155,33.6458333401613,48.706329375));
#8910=CARTESIAN_POINT('Ctrl Pts',(-9.95098946405443E-15,33.437500006828,
48.706329375));
#8911=CARTESIAN_POINT('Ctrl Pts',(-13.0508216223155,33.2291666734946,48.706329375));
#8912=CARTESIAN_POINT('Ctrl Pts',(-24.3531646875,33.0208333401613,42.1809185638423));
#8913=CARTESIAN_POINT('Ctrl Pts',(-35.6555077526845,32.812500006828,35.6555077526845));
#8914=CARTESIAN_POINT('Ctrl Pts',(-42.1809185638422,32.6041666734946,24.3531646875));
#8915=CARTESIAN_POINT('Ctrl Pts',(-48.706329375,32.3958333401613,13.0508216223155));
#8916=CARTESIAN_POINT('Ctrl Pts',(-48.706329375,32.187500006828,-1.8898197019151E-14));
#8917=CARTESIAN_POINT('Ctrl Pts',(-48.706329375,31.9791666734946,-13.0508216223155));
#8918=CARTESIAN_POINT('Ctrl Pts',(-42.1809185638422,31.7708333401613,-24.3531646875));
#8919=CARTESIAN_POINT('Ctrl Pts',(-35.6555077526845,31.562500006828,-35.6555077526845));
#8920=CARTESIAN_POINT('Ctrl Pts',(-24.3531646875,31.3541666734946,-42.1809185638423));
#8921=CARTESIAN_POINT('Ctrl Pts',(-13.0508216223155,31.1458333401613,-48.706329375));
#8922=CARTESIAN_POINT('Ctrl Pts',(1.59157945007855E-14,30.937500006828,
-48.706329375));
#8923=CARTESIAN_POINT('Ctrl Pts',(13.0508216223155,30.7291666734946,-48.706329375));
#8924=CARTESIAN_POINT('Ctrl Pts',(24.3531646875,30.5208333401613,-42.1809185638422));
#8925=CARTESIAN_POINT('Ctrl Pts',(35.6555077526845,30.312500006828,-35.6555077526845));
#8926=CARTESIAN_POINT('Ctrl Pts',(42.1809185638422,30.1041666734946,-24.3531646875));
#8927=CARTESIAN_POINT('Ctrl Pts',(48.706329375,29.8958333401613,-13.0508216223155));
#8928=CARTESIAN_POINT('Ctrl Pts',(48.706329375,29.687500006828,1.293339198242E-14));
#8929=CARTESIAN_POINT('Ctrl Pts',(48.706329375,29.4791666734946,13.0508216223155));
#8930=CARTESIAN_POINT('Ctrl Pts',(42.1809185638422,29.2708333401613,24.3531646875));
#8931=CARTESIAN_POINT('Ctrl Pts',(35.6555077526845,29.062500006828,35.6555077526845));
#8932=CARTESIAN_POINT('Ctrl Pts',(24.3531646875,28.8541666734946,42.1809185638422));
#8933=CARTESIAN_POINT('Ctrl Pts',(13.0508216223155,28.6458333401613,48.706329375));
#8934=CARTESIAN_POINT('Ctrl Pts',(-9.95098946405443E-15,28.437500006828,
48.706329375));
#8935=CARTESIAN_POINT('Ctrl Pts',(-13.0508216223155,28.2291666734946,48.706329375));
#8936=CARTESIAN_POINT('Ctrl Pts',(-24.3531646875,28.0208333401613,42.1809185638423));
#8937=CARTESIAN_POINT('Ctrl Pts',(-35.6555077526845,27.812500006828,35.6555077526845));
#8938=CARTESIAN_POINT('Ctrl Pts',(-42.1809185638422,27.6041666734946,24.3531646875));
#8939=CARTESIAN_POINT('Ctrl Pts',(-48.706329375,27.3958333401613,13.0508216223155));
#8940=CARTESIAN_POINT('Ctrl Pts',(-48.706329375,27.187500006828,-1.8898197019151E-14));
#8941=CARTESIAN_POINT('',(-4.32456003949878,53.3676432269777,48.5139639861634));
#8942=CARTESIAN_POINT('',(-48.5725845633798,52.2456516907297,3.60701400320327));
#8943=CARTESIAN_POINT('Ctrl Pts',(-4.32456003949878,53.3676432269777,48.5139639861634));
#8944=CARTESIAN_POINT('Ctrl Pts',(-15.038141415499,53.1925348924095,47.5589497574396));
#8945=CARTESIAN_POINT('Ctrl Pts',(-24.3531646875,53.0208333401613,42.1809185638423));
#8946=CARTESIAN_POINT('Ctrl Pts',(-35.6555077526845,52.812500006828,35.6555077526845));
#8947=CARTESIAN_POINT('Ctrl Pts',(-42.1809185638422,52.6041666734946,24.3531646875));
#8948=CARTESIAN_POINT('Ctrl Pts',(-47.7480251419551,52.4264286116309,14.7106532430575));
#8949=CARTESIAN_POINT('Ctrl Pts',(-48.5725845633798,52.2456516907297,3.60701400320327));
#8950=CARTESIAN_POINT('Ctrl Pts',(-48.5725845633798,52.2456516907297,3.60701400320327));
#8951=CARTESIAN_POINT('Ctrl Pts',(-48.3407853679392,52.1124685639422,3.60701400320327));
#8952=CARTESIAN_POINT('Ctrl Pts',(-48.1089821836664,51.9792923792741,3.60701400320327));
#8953=CARTESIAN_POINT('Ctrl Pts',(-47.6453674864979,51.7129545080418,3.60701400320327));
#8954=CARTESIAN_POINT('Ctrl Pts',(-47.4135559734253,51.5797928212585,3.60701400320325));
#8955=CARTESIAN_POINT('Ctrl Pts',(-47.1817401099609,51.4466387085919,3.60701400320325));
#8956=CARTESIAN_POINT('Ctrl Pts',(-46.7406305897488,51.1932671494809,3.60701400320325));
#8957=CARTESIAN_POINT('Ctrl Pts',(-46.2995053259033,50.9399229970588,3.60701400320327));
#8958=CARTESIAN_POINT('Ctrl Pts',(-45.858362923034,50.686608693912,3.60701400320327));
#8959=CARTESIAN_POINT('Ctrl Pts',(-4.32456003949877,51.8009818542622,45.7962681936506));
#8960=CARTESIAN_POINT('Ctrl Pts',(-4.32456003949877,51.9344874667937,46.0278818021281));
#8961=CARTESIAN_POINT('Ctrl Pts',(-4.32456003949885,52.2015035419424,46.4911062234486));
#8962=CARTESIAN_POINT('Ctrl Pts',(-4.32456003949878,52.4685288945405,46.954325296818));
#8963=CARTESIAN_POINT('Ctrl Pts',(-4.32456003949878,52.8572357107336,47.6286149142205));
#8964=CARTESIAN_POINT('Ctrl Pts',(-4.32456003949878,53.1124357360102,48.0712916022845));
#8965=CARTESIAN_POINT('Ctrl Pts',(-4.32456003949878,53.3676432269777,48.5139639861634));
#8966=CARTESIAN_POINT('Ctrl Pts',(-46.,55.6250000136559,0.));
#8967=CARTESIAN_POINT('Ctrl Pts',(-46.,55.4166666803226,-12.3256628518316));
#8968=CARTESIAN_POINT('Ctrl Pts',(-39.8371685740842,55.2083333469893,-23.));
#8969=CARTESIAN_POINT('Ctrl Pts',(-33.6743371481684,55.0000000136559,-33.6743371481684));
#8970=CARTESIAN_POINT('Ctrl Pts',(-23.,54.7916666803226,-39.8371685740842));
#8971=CARTESIAN_POINT('Ctrl Pts',(-12.3256628518317,54.5833333469893,-46.));
#8972=CARTESIAN_POINT('Ctrl Pts',(-2.81668763803891E-15,54.3750000136559,
-46.));
#8973=CARTESIAN_POINT('Ctrl Pts',(12.3256628518316,54.1666666803226,-46.));
#8974=CARTESIAN_POINT('Ctrl Pts',(23.,53.9583333469893,-39.8371685740842));
#8975=CARTESIAN_POINT('Ctrl Pts',(33.6743371481683,53.7500000136559,-33.6743371481684));
#8976=CARTESIAN_POINT('Ctrl Pts',(39.8371685740842,53.5416666803226,-23.));
#8977=CARTESIAN_POINT('Ctrl Pts',(46.,53.3333333469893,-12.3256628518317));
#8978=CARTESIAN_POINT('Ctrl Pts',(46.,53.1250000136559,-5.63337527607782E-15));
#8979=CARTESIAN_POINT('Ctrl Pts',(46.,52.9166666803226,12.3256628518316));
#8980=CARTESIAN_POINT('Ctrl Pts',(39.8371685740842,52.7083333469893,23.));
#8981=CARTESIAN_POINT('Ctrl Pts',(33.6743371481684,52.5000000136559,33.6743371481683));
#8982=CARTESIAN_POINT('Ctrl Pts',(23.,52.2916666803226,39.8371685740842));
#8983=CARTESIAN_POINT('Ctrl Pts',(12.3256628518317,52.0833333469893,46.));
#8984=CARTESIAN_POINT('Ctrl Pts',(8.45006291411674E-15,51.8750000136559,
46.));
#8985=CARTESIAN_POINT('Ctrl Pts',(-12.3256628518316,51.6666666803226,46.));
#8986=CARTESIAN_POINT('Ctrl Pts',(-23.,51.4583333469893,39.8371685740842));
#8987=CARTESIAN_POINT('Ctrl Pts',(-33.6743371481683,51.2500000136559,33.6743371481684));
#8988=CARTESIAN_POINT('Ctrl Pts',(-39.8371685740842,51.0416666803226,23.));
#8989=CARTESIAN_POINT('Ctrl Pts',(-46.,50.8333333469893,12.3256628518317));
#8990=CARTESIAN_POINT('Ctrl Pts',(-46.,50.6250000136559,0.));
#8991=CARTESIAN_POINT('Ctrl Pts',(-46.,50.4166666803226,-12.3256628518316));
#8992=CARTESIAN_POINT('Ctrl Pts',(-39.8371685740842,50.2083333469893,-23.));
#8993=CARTESIAN_POINT('Ctrl Pts',(-33.6743371481684,50.0000000136559,-33.6743371481684));
#8994=CARTESIAN_POINT('Ctrl Pts',(-23.,49.7916666803226,-39.8371685740842));
#8995=CARTESIAN_POINT('Ctrl Pts',(-12.3256628518317,49.5833333469893,-46.));
#8996=CARTESIAN_POINT('Ctrl Pts',(-2.81668763803891E-15,49.3750000136559,
-46.));
#8997=CARTESIAN_POINT('Ctrl Pts',(12.3256628518316,49.1666666803226,-46.));
#8998=CARTESIAN_POINT('Ctrl Pts',(23.,48.9583333469893,-39.8371685740842));
#8999=CARTESIAN_POINT('Ctrl Pts',(33.6743371481683,48.7500000136559,-33.6743371481684));
#9000=CARTESIAN_POINT('Ctrl Pts',(39.8371685740842,48.5416666803226,-23.));
#9001=CARTESIAN_POINT('Ctrl Pts',(46.,48.3333333469893,-12.3256628518317));
#9002=CARTESIAN_POINT('Ctrl Pts',(46.,48.1250000136559,-5.63337527607782E-15));
#9003=CARTESIAN_POINT('Ctrl Pts',(46.,47.9166666803226,12.3256628518316));
#9004=CARTESIAN_POINT('Ctrl Pts',(39.8371685740842,47.7083333469893,23.));
#9005=CARTESIAN_POINT('Ctrl Pts',(33.6743371481684,47.5000000136559,33.6743371481683));
#9006=CARTESIAN_POINT('Ctrl Pts',(23.,47.2916666803226,39.8371685740842));
#9007=CARTESIAN_POINT('Ctrl Pts',(12.3256628518317,47.0833333469893,46.));
#9008=CARTESIAN_POINT('Ctrl Pts',(8.45006291411674E-15,46.8750000136559,
46.));
#9009=CARTESIAN_POINT('Ctrl Pts',(-12.3256628518316,46.6666666803226,46.));
#9010=CARTESIAN_POINT('Ctrl Pts',(-23.,46.4583333469893,39.8371685740842));
#9011=CARTESIAN_POINT('Ctrl Pts',(-33.6743371481683,46.2500000136559,33.6743371481684));
#9012=CARTESIAN_POINT('Ctrl Pts',(-39.8371685740842,46.0416666803226,23.));
#9013=CARTESIAN_POINT('Ctrl Pts',(-46.,45.8333333469892,12.3256628518317));
#9014=CARTESIAN_POINT('Ctrl Pts',(-46.,45.6250000136559,0.));
#9015=CARTESIAN_POINT('Ctrl Pts',(-46.,45.4166666803226,-12.3256628518316));
#9016=CARTESIAN_POINT('Ctrl Pts',(-39.8371685740842,45.2083333469893,-23.));
#9017=CARTESIAN_POINT('Ctrl Pts',(-33.6743371481684,45.0000000136559,-33.6743371481684));
#9018=CARTESIAN_POINT('Ctrl Pts',(-23.,44.7916666803226,-39.8371685740842));
#9019=CARTESIAN_POINT('Ctrl Pts',(-12.3256628518317,44.5833333469893,-46.));
#9020=CARTESIAN_POINT('Ctrl Pts',(-2.81668763803891E-15,44.3750000136559,
-46.));
#9021=CARTESIAN_POINT('Ctrl Pts',(12.3256628518316,44.1666666803226,-46.));
#9022=CARTESIAN_POINT('Ctrl Pts',(23.,43.9583333469893,-39.8371685740842));
#9023=CARTESIAN_POINT('Ctrl Pts',(33.6743371481683,43.7500000136559,-33.6743371481684));
#9024=CARTESIAN_POINT('Ctrl Pts',(39.8371685740842,43.5416666803226,-23.));
#9025=CARTESIAN_POINT('Ctrl Pts',(46.,43.3333333469893,-12.3256628518317));
#9026=CARTESIAN_POINT('Ctrl Pts',(46.,43.1250000136559,-5.63337527607782E-15));
#9027=CARTESIAN_POINT('Ctrl Pts',(46.,42.9166666803226,12.3256628518316));
#9028=CARTESIAN_POINT('Ctrl Pts',(39.8371685740842,42.7083333469893,23.));
#9029=CARTESIAN_POINT('Ctrl Pts',(33.6743371481684,42.5000000136559,33.6743371481683));
#9030=CARTESIAN_POINT('Ctrl Pts',(23.,42.2916666803226,39.8371685740842));
#9031=CARTESIAN_POINT('Ctrl Pts',(12.3256628518317,42.0833333469893,46.));
#9032=CARTESIAN_POINT('Ctrl Pts',(8.45006291411674E-15,41.8750000136559,
46.));
#9033=CARTESIAN_POINT('Ctrl Pts',(-12.3256628518316,41.6666666803226,46.));
#9034=CARTESIAN_POINT('Ctrl Pts',(-23.,41.4583333469893,39.8371685740842));
#9035=CARTESIAN_POINT('Ctrl Pts',(-33.6743371481683,41.2500000136559,33.6743371481684));
#9036=CARTESIAN_POINT('Ctrl Pts',(-39.8371685740842,41.0416666803226,23.));
#9037=CARTESIAN_POINT('Ctrl Pts',(-46.,40.8333333469893,12.3256628518317));
#9038=CARTESIAN_POINT('Ctrl Pts',(-46.,40.6250000136559,0.));
#9039=CARTESIAN_POINT('Ctrl Pts',(-46.,40.4166666803226,-12.3256628518316));
#9040=CARTESIAN_POINT('Ctrl Pts',(-39.8371685740842,40.2083333469893,-23.));
#9041=CARTESIAN_POINT('Ctrl Pts',(-33.6743371481684,40.0000000136559,-33.6743371481684));
#9042=CARTESIAN_POINT('Ctrl Pts',(-23.,39.7916666803226,-39.8371685740842));
#9043=CARTESIAN_POINT('Ctrl Pts',(-12.3256628518317,39.5833333469893,-46.));
#9044=CARTESIAN_POINT('Ctrl Pts',(-2.81668763803891E-15,39.3750000136559,
-46.));
#9045=CARTESIAN_POINT('Ctrl Pts',(12.3256628518316,39.1666666803226,-46.));
#9046=CARTESIAN_POINT('Ctrl Pts',(23.,38.9583333469893,-39.8371685740842));
#9047=CARTESIAN_POINT('Ctrl Pts',(33.6743371481683,38.7500000136559,-33.6743371481684));
#9048=CARTESIAN_POINT('Ctrl Pts',(39.8371685740842,38.5416666803226,-23.));
#9049=CARTESIAN_POINT('Ctrl Pts',(46.,38.3333333469893,-12.3256628518317));
#9050=CARTESIAN_POINT('Ctrl Pts',(46.,38.1250000136559,-5.63337527607782E-15));
#9051=CARTESIAN_POINT('Ctrl Pts',(46.,37.9166666803226,12.3256628518316));
#9052=CARTESIAN_POINT('Ctrl Pts',(39.8371685740842,37.7083333469893,23.));
#9053=CARTESIAN_POINT('Ctrl Pts',(33.6743371481684,37.5000000136559,33.6743371481683));
#9054=CARTESIAN_POINT('Ctrl Pts',(23.,37.2916666803226,39.8371685740842));
#9055=CARTESIAN_POINT('Ctrl Pts',(12.3256628518317,37.0833333469893,46.));
#9056=CARTESIAN_POINT('Ctrl Pts',(8.45006291411674E-15,36.8750000136559,
46.));
#9057=CARTESIAN_POINT('Ctrl Pts',(-12.3256628518316,36.6666666803226,46.));
#9058=CARTESIAN_POINT('Ctrl Pts',(-23.,36.4583333469893,39.8371685740842));
#9059=CARTESIAN_POINT('Ctrl Pts',(-33.6743371481683,36.2500000136559,33.6743371481684));
#9060=CARTESIAN_POINT('Ctrl Pts',(-39.8371685740842,36.0416666803226,23.));
#9061=CARTESIAN_POINT('Ctrl Pts',(-46.,35.8333333469893,12.3256628518317));
#9062=CARTESIAN_POINT('Ctrl Pts',(-46.,35.6250000136559,0.));
#9063=CARTESIAN_POINT('Ctrl Pts',(-46.,35.4166666803226,-12.3256628518316));
#9064=CARTESIAN_POINT('Ctrl Pts',(-39.8371685740842,35.2083333469893,-23.));
#9065=CARTESIAN_POINT('Ctrl Pts',(-33.6743371481684,35.0000000136559,-33.6743371481684));
#9066=CARTESIAN_POINT('Ctrl Pts',(-23.,34.7916666803226,-39.8371685740842));
#9067=CARTESIAN_POINT('Ctrl Pts',(-12.3256628518317,34.5833333469893,-46.));
#9068=CARTESIAN_POINT('Ctrl Pts',(-2.81668763803891E-15,34.3750000136559,
-46.));
#9069=CARTESIAN_POINT('Ctrl Pts',(12.3256628518316,34.1666666803226,-46.));
#9070=CARTESIAN_POINT('Ctrl Pts',(23.,33.9583333469893,-39.8371685740842));
#9071=CARTESIAN_POINT('Ctrl Pts',(33.6743371481683,33.7500000136559,-33.6743371481684));
#9072=CARTESIAN_POINT('Ctrl Pts',(39.8371685740842,33.5416666803226,-23.));
#9073=CARTESIAN_POINT('Ctrl Pts',(46.,33.3333333469893,-12.3256628518317));
#9074=CARTESIAN_POINT('Ctrl Pts',(46.,33.1250000136559,-5.63337527607782E-15));
#9075=CARTESIAN_POINT('Ctrl Pts',(46.,32.9166666803226,12.3256628518316));
#9076=CARTESIAN_POINT('Ctrl Pts',(39.8371685740842,32.7083333469893,23.));
#9077=CARTESIAN_POINT('Ctrl Pts',(33.6743371481684,32.5000000136559,33.6743371481683));
#9078=CARTESIAN_POINT('Ctrl Pts',(23.,32.2916666803226,39.8371685740842));
#9079=CARTESIAN_POINT('Ctrl Pts',(12.3256628518317,32.0833333469893,46.));
#9080=CARTESIAN_POINT('Ctrl Pts',(8.45006291411674E-15,31.8750000136559,
46.));
#9081=CARTESIAN_POINT('Ctrl Pts',(-12.3256628518316,31.6666666803226,46.));
#9082=CARTESIAN_POINT('Ctrl Pts',(-23.,31.4583333469893,39.8371685740842));
#9083=CARTESIAN_POINT('Ctrl Pts',(-33.6743371481683,31.2500000136559,33.6743371481684));
#9084=CARTESIAN_POINT('Ctrl Pts',(-39.8371685740842,31.0416666803226,23.));
#9085=CARTESIAN_POINT('Ctrl Pts',(-46.,30.8333333469893,12.3256628518317));
#9086=CARTESIAN_POINT('Ctrl Pts',(-46.,30.6250000136559,0.));
#9087=CARTESIAN_POINT('Ctrl Pts',(-46.,30.4166666803226,-12.3256628518316));
#9088=CARTESIAN_POINT('Ctrl Pts',(-39.8371685740842,30.2083333469893,-23.));
#9089=CARTESIAN_POINT('Ctrl Pts',(-33.6743371481684,30.0000000136559,-33.6743371481684));
#9090=CARTESIAN_POINT('Ctrl Pts',(-23.,29.7916666803226,-39.8371685740842));
#9091=CARTESIAN_POINT('Ctrl Pts',(-12.3256628518317,29.5833333469893,-46.));
#9092=CARTESIAN_POINT('Ctrl Pts',(-2.81668763803891E-15,29.3750000136559,
-46.));
#9093=CARTESIAN_POINT('Ctrl Pts',(12.3256628518316,29.1666666803226,-46.));
#9094=CARTESIAN_POINT('Ctrl Pts',(23.,28.9583333469893,-39.8371685740842));
#9095=CARTESIAN_POINT('Ctrl Pts',(33.6743371481683,28.7500000136559,-33.6743371481684));
#9096=CARTESIAN_POINT('Ctrl Pts',(39.8371685740842,28.5416666803226,-23.));
#9097=CARTESIAN_POINT('Ctrl Pts',(46.,28.3333333469893,-12.3256628518317));
#9098=CARTESIAN_POINT('Ctrl Pts',(46.,28.1250000136559,-5.63337527607782E-15));
#9099=CARTESIAN_POINT('Ctrl Pts',(46.,27.9166666803226,12.3256628518316));
#9100=CARTESIAN_POINT('Ctrl Pts',(39.8371685740842,27.7083333469893,23.));
#9101=CARTESIAN_POINT('Ctrl Pts',(33.6743371481684,27.5000000136559,33.6743371481683));
#9102=CARTESIAN_POINT('Ctrl Pts',(23.,27.2916666803226,39.8371685740842));
#9103=CARTESIAN_POINT('Ctrl Pts',(12.3256628518317,27.0833333469893,46.));
#9104=CARTESIAN_POINT('Ctrl Pts',(8.45006291411674E-15,26.8750000136559,
46.));
#9105=CARTESIAN_POINT('Ctrl Pts',(-12.3256628518316,26.6666666803226,46.));
#9106=CARTESIAN_POINT('Ctrl Pts',(-23.,26.4583333469893,39.8371685740842));
#9107=CARTESIAN_POINT('Ctrl Pts',(-33.6743371481683,26.2500000136559,33.6743371481684));
#9108=CARTESIAN_POINT('Ctrl Pts',(-39.8371685740842,26.0416666803226,23.));
#9109=CARTESIAN_POINT('Ctrl Pts',(-46.,25.8333333469893,12.3256628518317));
#9110=CARTESIAN_POINT('Ctrl Pts',(-46.,25.6250000136559,0.));
#9111=CARTESIAN_POINT('Ctrl Pts',(-48.706329375,57.187500006828,-1.8898197019151E-14));
#9112=CARTESIAN_POINT('Ctrl Pts',(-48.706329375,56.9791666734946,-13.0508216223155));
#9113=CARTESIAN_POINT('Ctrl Pts',(-42.1809185638422,56.7708333401613,-24.3531646875));
#9114=CARTESIAN_POINT('Ctrl Pts',(-35.6555077526845,56.562500006828,-35.6555077526845));
#9115=CARTESIAN_POINT('Ctrl Pts',(-24.3531646875,56.3541666734946,-42.1809185638423));
#9116=CARTESIAN_POINT('Ctrl Pts',(-13.0508216223155,56.1458333401613,-48.706329375));
#9117=CARTESIAN_POINT('Ctrl Pts',(1.59157945007855E-14,55.937500006828,
-48.706329375));
#9118=CARTESIAN_POINT('Ctrl Pts',(13.0508216223155,55.7291666734946,-48.706329375));
#9119=CARTESIAN_POINT('Ctrl Pts',(24.3531646875,55.5208333401613,-42.1809185638422));
#9120=CARTESIAN_POINT('Ctrl Pts',(35.6555077526845,55.312500006828,-35.6555077526845));
#9121=CARTESIAN_POINT('Ctrl Pts',(42.1809185638422,55.1041666734946,-24.3531646875));
#9122=CARTESIAN_POINT('Ctrl Pts',(48.706329375,54.8958333401613,-13.0508216223155));
#9123=CARTESIAN_POINT('Ctrl Pts',(48.706329375,54.687500006828,1.293339198242E-14));
#9124=CARTESIAN_POINT('Ctrl Pts',(48.706329375,54.4791666734946,13.0508216223155));
#9125=CARTESIAN_POINT('Ctrl Pts',(42.1809185638422,54.2708333401613,24.3531646875));
#9126=CARTESIAN_POINT('Ctrl Pts',(35.6555077526845,54.062500006828,35.6555077526845));
#9127=CARTESIAN_POINT('Ctrl Pts',(24.3531646875,53.8541666734946,42.1809185638422));
#9128=CARTESIAN_POINT('Ctrl Pts',(13.0508216223155,53.6458333401613,48.706329375));
#9129=CARTESIAN_POINT('Ctrl Pts',(-9.95098946405443E-15,53.437500006828,
48.706329375));
#9130=CARTESIAN_POINT('Ctrl Pts',(-13.0508216223155,53.2291666734946,48.706329375));
#9131=CARTESIAN_POINT('Ctrl Pts',(-24.3531646875,53.0208333401613,42.1809185638423));
#9132=CARTESIAN_POINT('Ctrl Pts',(-35.6555077526845,52.812500006828,35.6555077526845));
#9133=CARTESIAN_POINT('Ctrl Pts',(-42.1809185638422,52.6041666734946,24.3531646875));
#9134=CARTESIAN_POINT('Ctrl Pts',(-48.706329375,52.3958333401613,13.0508216223155));
#9135=CARTESIAN_POINT('Ctrl Pts',(-48.706329375,52.187500006828,-1.8898197019151E-14));
#9136=CARTESIAN_POINT('Ctrl Pts',(-48.706329375,51.9791666734946,-13.0508216223155));
#9137=CARTESIAN_POINT('Ctrl Pts',(-42.1809185638422,51.7708333401613,-24.3531646875));
#9138=CARTESIAN_POINT('Ctrl Pts',(-35.6555077526845,51.562500006828,-35.6555077526845));
#9139=CARTESIAN_POINT('Ctrl Pts',(-24.3531646875,51.3541666734946,-42.1809185638423));
#9140=CARTESIAN_POINT('Ctrl Pts',(-13.0508216223155,51.1458333401613,-48.706329375));
#9141=CARTESIAN_POINT('Ctrl Pts',(1.59157945007855E-14,50.937500006828,
-48.706329375));
#9142=CARTESIAN_POINT('Ctrl Pts',(13.0508216223155,50.7291666734946,-48.706329375));
#9143=CARTESIAN_POINT('Ctrl Pts',(24.3531646875,50.5208333401613,-42.1809185638422));
#9144=CARTESIAN_POINT('Ctrl Pts',(35.6555077526845,50.312500006828,-35.6555077526845));
#9145=CARTESIAN_POINT('Ctrl Pts',(42.1809185638422,50.1041666734946,-24.3531646875));
#9146=CARTESIAN_POINT('Ctrl Pts',(48.706329375,49.8958333401613,-13.0508216223155));
#9147=CARTESIAN_POINT('Ctrl Pts',(48.706329375,49.687500006828,1.293339198242E-14));
#9148=CARTESIAN_POINT('Ctrl Pts',(48.706329375,49.4791666734946,13.0508216223155));
#9149=CARTESIAN_POINT('Ctrl Pts',(42.1809185638422,49.2708333401613,24.3531646875));
#9150=CARTESIAN_POINT('Ctrl Pts',(35.6555077526845,49.062500006828,35.6555077526845));
#9151=CARTESIAN_POINT('Ctrl Pts',(24.3531646875,48.8541666734946,42.1809185638422));
#9152=CARTESIAN_POINT('Ctrl Pts',(13.0508216223155,48.6458333401613,48.706329375));
#9153=CARTESIAN_POINT('Ctrl Pts',(-9.95098946405443E-15,48.437500006828,
48.706329375));
#9154=CARTESIAN_POINT('Ctrl Pts',(-13.0508216223155,48.2291666734946,48.706329375));
#9155=CARTESIAN_POINT('Ctrl Pts',(-24.3531646875,48.0208333401613,42.1809185638423));
#9156=CARTESIAN_POINT('Ctrl Pts',(-35.6555077526845,47.812500006828,35.6555077526845));
#9157=CARTESIAN_POINT('Ctrl Pts',(-42.1809185638422,47.6041666734946,24.3531646875));
#9158=CARTESIAN_POINT('Ctrl Pts',(-48.706329375,47.3958333401613,13.0508216223155));
#9159=CARTESIAN_POINT('Ctrl Pts',(-48.706329375,47.187500006828,-1.8898197019151E-14));
#9160=CARTESIAN_POINT('Ctrl Pts',(-48.706329375,46.9791666734946,-13.0508216223155));
#9161=CARTESIAN_POINT('Ctrl Pts',(-42.1809185638422,46.7708333401613,-24.3531646875));
#9162=CARTESIAN_POINT('Ctrl Pts',(-35.6555077526845,46.562500006828,-35.6555077526845));
#9163=CARTESIAN_POINT('Ctrl Pts',(-24.3531646875,46.3541666734946,-42.1809185638423));
#9164=CARTESIAN_POINT('Ctrl Pts',(-13.0508216223155,46.1458333401613,-48.706329375));
#9165=CARTESIAN_POINT('Ctrl Pts',(1.59157945007855E-14,45.937500006828,
-48.706329375));
#9166=CARTESIAN_POINT('Ctrl Pts',(13.0508216223155,45.7291666734946,-48.706329375));
#9167=CARTESIAN_POINT('Ctrl Pts',(24.3531646875,45.5208333401613,-42.1809185638422));
#9168=CARTESIAN_POINT('Ctrl Pts',(35.6555077526845,45.312500006828,-35.6555077526845));
#9169=CARTESIAN_POINT('Ctrl Pts',(42.1809185638422,45.1041666734946,-24.3531646875));
#9170=CARTESIAN_POINT('Ctrl Pts',(48.706329375,44.8958333401613,-13.0508216223155));
#9171=CARTESIAN_POINT('Ctrl Pts',(48.706329375,44.687500006828,1.293339198242E-14));
#9172=CARTESIAN_POINT('Ctrl Pts',(48.706329375,44.4791666734946,13.0508216223155));
#9173=CARTESIAN_POINT('Ctrl Pts',(42.1809185638422,44.2708333401613,24.3531646875));
#9174=CARTESIAN_POINT('Ctrl Pts',(35.6555077526845,44.062500006828,35.6555077526845));
#9175=CARTESIAN_POINT('Ctrl Pts',(24.3531646875,43.8541666734946,42.1809185638422));
#9176=CARTESIAN_POINT('Ctrl Pts',(13.0508216223155,43.6458333401613,48.706329375));
#9177=CARTESIAN_POINT('Ctrl Pts',(-9.95098946405443E-15,43.437500006828,
48.706329375));
#9178=CARTESIAN_POINT('Ctrl Pts',(-13.0508216223155,43.2291666734946,48.706329375));
#9179=CARTESIAN_POINT('Ctrl Pts',(-24.3531646875,43.0208333401613,42.1809185638423));
#9180=CARTESIAN_POINT('Ctrl Pts',(-35.6555077526845,42.812500006828,35.6555077526845));
#9181=CARTESIAN_POINT('Ctrl Pts',(-42.1809185638422,42.6041666734946,24.3531646875));
#9182=CARTESIAN_POINT('Ctrl Pts',(-48.706329375,42.3958333401613,13.0508216223155));
#9183=CARTESIAN_POINT('Ctrl Pts',(-48.706329375,42.187500006828,-1.8898197019151E-14));
#9184=CARTESIAN_POINT('Ctrl Pts',(-48.706329375,41.9791666734946,-13.0508216223155));
#9185=CARTESIAN_POINT('Ctrl Pts',(-42.1809185638422,41.7708333401613,-24.3531646875));
#9186=CARTESIAN_POINT('Ctrl Pts',(-35.6555077526845,41.562500006828,-35.6555077526845));
#9187=CARTESIAN_POINT('Ctrl Pts',(-24.3531646875,41.3541666734946,-42.1809185638423));
#9188=CARTESIAN_POINT('Ctrl Pts',(-13.0508216223155,41.1458333401613,-48.706329375));
#9189=CARTESIAN_POINT('Ctrl Pts',(1.59157945007855E-14,40.937500006828,
-48.706329375));
#9190=CARTESIAN_POINT('Ctrl Pts',(13.0508216223155,40.7291666734946,-48.706329375));
#9191=CARTESIAN_POINT('Ctrl Pts',(24.3531646875,40.5208333401613,-42.1809185638422));
#9192=CARTESIAN_POINT('Ctrl Pts',(35.6555077526845,40.312500006828,-35.6555077526845));
#9193=CARTESIAN_POINT('Ctrl Pts',(42.1809185638422,40.1041666734946,-24.3531646875));
#9194=CARTESIAN_POINT('Ctrl Pts',(48.706329375,39.8958333401613,-13.0508216223155));
#9195=CARTESIAN_POINT('Ctrl Pts',(48.706329375,39.687500006828,1.293339198242E-14));
#9196=CARTESIAN_POINT('Ctrl Pts',(48.706329375,39.4791666734946,13.0508216223155));
#9197=CARTESIAN_POINT('Ctrl Pts',(42.1809185638422,39.2708333401613,24.3531646875));
#9198=CARTESIAN_POINT('Ctrl Pts',(35.6555077526845,39.062500006828,35.6555077526845));
#9199=CARTESIAN_POINT('Ctrl Pts',(24.3531646875,38.8541666734946,42.1809185638422));
#9200=CARTESIAN_POINT('Ctrl Pts',(13.0508216223155,38.6458333401613,48.706329375));
#9201=CARTESIAN_POINT('Ctrl Pts',(-9.95098946405443E-15,38.437500006828,
48.706329375));
#9202=CARTESIAN_POINT('Ctrl Pts',(-13.0508216223155,38.2291666734946,48.706329375));
#9203=CARTESIAN_POINT('Ctrl Pts',(-24.3531646875,38.0208333401613,42.1809185638423));
#9204=CARTESIAN_POINT('Ctrl Pts',(-35.6555077526845,37.812500006828,35.6555077526845));
#9205=CARTESIAN_POINT('Ctrl Pts',(-42.1809185638422,37.6041666734946,24.3531646875));
#9206=CARTESIAN_POINT('Ctrl Pts',(-48.706329375,37.3958333401613,13.0508216223155));
#9207=CARTESIAN_POINT('Ctrl Pts',(-48.706329375,37.187500006828,-1.8898197019151E-14));
#9208=CARTESIAN_POINT('Ctrl Pts',(-48.706329375,36.9791666734946,-13.0508216223155));
#9209=CARTESIAN_POINT('Ctrl Pts',(-42.1809185638422,36.7708333401613,-24.3531646875));
#9210=CARTESIAN_POINT('Ctrl Pts',(-35.6555077526845,36.562500006828,-35.6555077526845));
#9211=CARTESIAN_POINT('Ctrl Pts',(-24.3531646875,36.3541666734946,-42.1809185638423));
#9212=CARTESIAN_POINT('Ctrl Pts',(-13.0508216223155,36.1458333401613,-48.706329375));
#9213=CARTESIAN_POINT('Ctrl Pts',(1.59157945007855E-14,35.937500006828,
-48.706329375));
#9214=CARTESIAN_POINT('Ctrl Pts',(13.0508216223155,35.7291666734946,-48.706329375));
#9215=CARTESIAN_POINT('Ctrl Pts',(24.3531646875,35.5208333401613,-42.1809185638422));
#9216=CARTESIAN_POINT('Ctrl Pts',(35.6555077526845,35.312500006828,-35.6555077526845));
#9217=CARTESIAN_POINT('Ctrl Pts',(42.1809185638422,35.1041666734946,-24.3531646875));
#9218=CARTESIAN_POINT('Ctrl Pts',(48.706329375,34.8958333401613,-13.0508216223155));
#9219=CARTESIAN_POINT('Ctrl Pts',(48.706329375,34.687500006828,1.293339198242E-14));
#9220=CARTESIAN_POINT('Ctrl Pts',(48.706329375,34.4791666734946,13.0508216223155));
#9221=CARTESIAN_POINT('Ctrl Pts',(42.1809185638422,34.2708333401613,24.3531646875));
#9222=CARTESIAN_POINT('Ctrl Pts',(35.6555077526845,34.062500006828,35.6555077526845));
#9223=CARTESIAN_POINT('Ctrl Pts',(24.3531646875,33.8541666734946,42.1809185638422));
#9224=CARTESIAN_POINT('Ctrl Pts',(13.0508216223155,33.6458333401613,48.706329375));
#9225=CARTESIAN_POINT('Ctrl Pts',(-9.95098946405443E-15,33.437500006828,
48.706329375));
#9226=CARTESIAN_POINT('Ctrl Pts',(-13.0508216223155,33.2291666734946,48.706329375));
#9227=CARTESIAN_POINT('Ctrl Pts',(-24.3531646875,33.0208333401613,42.1809185638423));
#9228=CARTESIAN_POINT('Ctrl Pts',(-35.6555077526845,32.812500006828,35.6555077526845));
#9229=CARTESIAN_POINT('Ctrl Pts',(-42.1809185638422,32.6041666734946,24.3531646875));
#9230=CARTESIAN_POINT('Ctrl Pts',(-48.706329375,32.3958333401613,13.0508216223155));
#9231=CARTESIAN_POINT('Ctrl Pts',(-48.706329375,32.187500006828,-1.8898197019151E-14));
#9232=CARTESIAN_POINT('Ctrl Pts',(-48.706329375,31.9791666734946,-13.0508216223155));
#9233=CARTESIAN_POINT('Ctrl Pts',(-42.1809185638422,31.7708333401613,-24.3531646875));
#9234=CARTESIAN_POINT('Ctrl Pts',(-35.6555077526845,31.562500006828,-35.6555077526845));
#9235=CARTESIAN_POINT('Ctrl Pts',(-24.3531646875,31.3541666734946,-42.1809185638423));
#9236=CARTESIAN_POINT('Ctrl Pts',(-13.0508216223155,31.1458333401613,-48.706329375));
#9237=CARTESIAN_POINT('Ctrl Pts',(1.59157945007855E-14,30.937500006828,
-48.706329375));
#9238=CARTESIAN_POINT('Ctrl Pts',(13.0508216223155,30.7291666734946,-48.706329375));
#9239=CARTESIAN_POINT('Ctrl Pts',(24.3531646875,30.5208333401613,-42.1809185638422));
#9240=CARTESIAN_POINT('Ctrl Pts',(35.6555077526845,30.312500006828,-35.6555077526845));
#9241=CARTESIAN_POINT('Ctrl Pts',(42.1809185638422,30.1041666734946,-24.3531646875));
#9242=CARTESIAN_POINT('Ctrl Pts',(48.706329375,29.8958333401613,-13.0508216223155));
#9243=CARTESIAN_POINT('Ctrl Pts',(48.706329375,29.687500006828,1.293339198242E-14));
#9244=CARTESIAN_POINT('Ctrl Pts',(48.706329375,29.4791666734946,13.0508216223155));
#9245=CARTESIAN_POINT('Ctrl Pts',(42.1809185638422,29.2708333401613,24.3531646875));
#9246=CARTESIAN_POINT('Ctrl Pts',(35.6555077526845,29.062500006828,35.6555077526845));
#9247=CARTESIAN_POINT('Ctrl Pts',(24.3531646875,28.8541666734946,42.1809185638422));
#9248=CARTESIAN_POINT('Ctrl Pts',(13.0508216223155,28.6458333401613,48.706329375));
#9249=CARTESIAN_POINT('Ctrl Pts',(-9.95098946405443E-15,28.437500006828,
48.706329375));
#9250=CARTESIAN_POINT('Ctrl Pts',(-13.0508216223155,28.2291666734946,48.706329375));
#9251=CARTESIAN_POINT('Ctrl Pts',(-24.3531646875,28.0208333401613,42.1809185638423));
#9252=CARTESIAN_POINT('Ctrl Pts',(-35.6555077526845,27.812500006828,35.6555077526845));
#9253=CARTESIAN_POINT('Ctrl Pts',(-42.1809185638422,27.6041666734946,24.3531646875));
#9254=CARTESIAN_POINT('Ctrl Pts',(-48.706329375,27.3958333401613,13.0508216223155));
#9255=CARTESIAN_POINT('Ctrl Pts',(-48.706329375,27.187500006828,-1.8898197019151E-14));
#9256=CARTESIAN_POINT('',(-48.5134353784345,47.1175463684955,-4.33048599679673));
#9257=CARTESIAN_POINT('Ctrl Pts',(-45.7957082162897,45.5508791552084,-4.33048599679673));
#9258=CARTESIAN_POINT('Ctrl Pts',(-46.027322302781,45.6843839384496,-4.33048599679671));
#9259=CARTESIAN_POINT('Ctrl Pts',(-46.4905476657728,45.9513983799647,-4.33048599679668));
#9260=CARTESIAN_POINT('Ctrl Pts',(-46.9537676533565,46.2184221466352,-4.33048599679674));
#9261=CARTESIAN_POINT('Ctrl Pts',(-47.6280672732222,46.6071316973962,-4.33048599679674));
#9262=CARTESIAN_POINT('Ctrl Pts',(-48.0707534890442,46.8623352807796,-4.33048599679674));
#9263=CARTESIAN_POINT('Ctrl Pts',(-48.5134353784345,47.1175463684955,-4.33048599679673));
#9264=CARTESIAN_POINT('',(-4.32456003949881,46.0073567866782,-48.5139639861634));
#9265=CARTESIAN_POINT('Ctrl Pts',(-48.5134353784345,47.1175463684955,-4.33048599679674));
#9266=CARTESIAN_POINT('Ctrl Pts',(-47.5573898704235,46.9424850907233,-15.0408432190651));
#9267=CARTESIAN_POINT('Ctrl Pts',(-42.1809185638422,46.7708333401613,-24.3531646875));
#9268=CARTESIAN_POINT('Ctrl Pts',(-35.6555077526845,46.562500006828,-35.6555077526845));
#9269=CARTESIAN_POINT('Ctrl Pts',(-24.3531646875,46.3541666734946,-42.1809185638423));
#9270=CARTESIAN_POINT('Ctrl Pts',(-15.0381414154991,46.1824651212465,-47.5589497574396));
#9271=CARTESIAN_POINT('Ctrl Pts',(-4.32456003949881,46.0073567866782,-48.5139639861634));
#9272=CARTESIAN_POINT('Origin',(-4.32455753660831,8017.20454015463,4524.01087370844));
#9273=CARTESIAN_POINT('Ctrl Pts',(-46.,55.6250000136559,0.));
#9274=CARTESIAN_POINT('Ctrl Pts',(-46.,55.4166666803226,-12.3256628518316));
#9275=CARTESIAN_POINT('Ctrl Pts',(-39.8371685740842,55.2083333469893,-23.));
#9276=CARTESIAN_POINT('Ctrl Pts',(-33.6743371481684,55.0000000136559,-33.6743371481684));
#9277=CARTESIAN_POINT('Ctrl Pts',(-23.,54.7916666803226,-39.8371685740842));
#9278=CARTESIAN_POINT('Ctrl Pts',(-12.3256628518317,54.5833333469893,-46.));
#9279=CARTESIAN_POINT('Ctrl Pts',(-2.81668763803891E-15,54.3750000136559,
-46.));
#9280=CARTESIAN_POINT('Ctrl Pts',(12.3256628518316,54.1666666803226,-46.));
#9281=CARTESIAN_POINT('Ctrl Pts',(23.,53.9583333469893,-39.8371685740842));
#9282=CARTESIAN_POINT('Ctrl Pts',(33.6743371481683,53.7500000136559,-33.6743371481684));
#9283=CARTESIAN_POINT('Ctrl Pts',(39.8371685740842,53.5416666803226,-23.));
#9284=CARTESIAN_POINT('Ctrl Pts',(46.,53.3333333469893,-12.3256628518317));
#9285=CARTESIAN_POINT('Ctrl Pts',(46.,53.1250000136559,-5.63337527607782E-15));
#9286=CARTESIAN_POINT('Ctrl Pts',(46.,52.9166666803226,12.3256628518316));
#9287=CARTESIAN_POINT('Ctrl Pts',(39.8371685740842,52.7083333469893,23.));
#9288=CARTESIAN_POINT('Ctrl Pts',(33.6743371481684,52.5000000136559,33.6743371481683));
#9289=CARTESIAN_POINT('Ctrl Pts',(23.,52.2916666803226,39.8371685740842));
#9290=CARTESIAN_POINT('Ctrl Pts',(12.3256628518317,52.0833333469893,46.));
#9291=CARTESIAN_POINT('Ctrl Pts',(8.45006291411674E-15,51.8750000136559,
46.));
#9292=CARTESIAN_POINT('Ctrl Pts',(-12.3256628518316,51.6666666803226,46.));
#9293=CARTESIAN_POINT('Ctrl Pts',(-23.,51.4583333469893,39.8371685740842));
#9294=CARTESIAN_POINT('Ctrl Pts',(-33.6743371481683,51.2500000136559,33.6743371481684));
#9295=CARTESIAN_POINT('Ctrl Pts',(-39.8371685740842,51.0416666803226,23.));
#9296=CARTESIAN_POINT('Ctrl Pts',(-46.,50.8333333469893,12.3256628518317));
#9297=CARTESIAN_POINT('Ctrl Pts',(-46.,50.6250000136559,0.));
#9298=CARTESIAN_POINT('Ctrl Pts',(-46.,50.4166666803226,-12.3256628518316));
#9299=CARTESIAN_POINT('Ctrl Pts',(-39.8371685740842,50.2083333469893,-23.));
#9300=CARTESIAN_POINT('Ctrl Pts',(-33.6743371481684,50.0000000136559,-33.6743371481684));
#9301=CARTESIAN_POINT('Ctrl Pts',(-23.,49.7916666803226,-39.8371685740842));
#9302=CARTESIAN_POINT('Ctrl Pts',(-12.3256628518317,49.5833333469893,-46.));
#9303=CARTESIAN_POINT('Ctrl Pts',(-2.81668763803891E-15,49.3750000136559,
-46.));
#9304=CARTESIAN_POINT('Ctrl Pts',(12.3256628518316,49.1666666803226,-46.));
#9305=CARTESIAN_POINT('Ctrl Pts',(23.,48.9583333469893,-39.8371685740842));
#9306=CARTESIAN_POINT('Ctrl Pts',(33.6743371481683,48.7500000136559,-33.6743371481684));
#9307=CARTESIAN_POINT('Ctrl Pts',(39.8371685740842,48.5416666803226,-23.));
#9308=CARTESIAN_POINT('Ctrl Pts',(46.,48.3333333469893,-12.3256628518317));
#9309=CARTESIAN_POINT('Ctrl Pts',(46.,48.1250000136559,-5.63337527607782E-15));
#9310=CARTESIAN_POINT('Ctrl Pts',(46.,47.9166666803226,12.3256628518316));
#9311=CARTESIAN_POINT('Ctrl Pts',(39.8371685740842,47.7083333469893,23.));
#9312=CARTESIAN_POINT('Ctrl Pts',(33.6743371481684,47.5000000136559,33.6743371481683));
#9313=CARTESIAN_POINT('Ctrl Pts',(23.,47.2916666803226,39.8371685740842));
#9314=CARTESIAN_POINT('Ctrl Pts',(12.3256628518317,47.0833333469893,46.));
#9315=CARTESIAN_POINT('Ctrl Pts',(8.45006291411674E-15,46.8750000136559,
46.));
#9316=CARTESIAN_POINT('Ctrl Pts',(-12.3256628518316,46.6666666803226,46.));
#9317=CARTESIAN_POINT('Ctrl Pts',(-23.,46.4583333469893,39.8371685740842));
#9318=CARTESIAN_POINT('Ctrl Pts',(-33.6743371481683,46.2500000136559,33.6743371481684));
#9319=CARTESIAN_POINT('Ctrl Pts',(-39.8371685740842,46.0416666803226,23.));
#9320=CARTESIAN_POINT('Ctrl Pts',(-46.,45.8333333469892,12.3256628518317));
#9321=CARTESIAN_POINT('Ctrl Pts',(-46.,45.6250000136559,0.));
#9322=CARTESIAN_POINT('Ctrl Pts',(-46.,45.4166666803226,-12.3256628518316));
#9323=CARTESIAN_POINT('Ctrl Pts',(-39.8371685740842,45.2083333469893,-23.));
#9324=CARTESIAN_POINT('Ctrl Pts',(-33.6743371481684,45.0000000136559,-33.6743371481684));
#9325=CARTESIAN_POINT('Ctrl Pts',(-23.,44.7916666803226,-39.8371685740842));
#9326=CARTESIAN_POINT('Ctrl Pts',(-12.3256628518317,44.5833333469893,-46.));
#9327=CARTESIAN_POINT('Ctrl Pts',(-2.81668763803891E-15,44.3750000136559,
-46.));
#9328=CARTESIAN_POINT('Ctrl Pts',(12.3256628518316,44.1666666803226,-46.));
#9329=CARTESIAN_POINT('Ctrl Pts',(23.,43.9583333469893,-39.8371685740842));
#9330=CARTESIAN_POINT('Ctrl Pts',(33.6743371481683,43.7500000136559,-33.6743371481684));
#9331=CARTESIAN_POINT('Ctrl Pts',(39.8371685740842,43.5416666803226,-23.));
#9332=CARTESIAN_POINT('Ctrl Pts',(46.,43.3333333469893,-12.3256628518317));
#9333=CARTESIAN_POINT('Ctrl Pts',(46.,43.1250000136559,-5.63337527607782E-15));
#9334=CARTESIAN_POINT('Ctrl Pts',(46.,42.9166666803226,12.3256628518316));
#9335=CARTESIAN_POINT('Ctrl Pts',(39.8371685740842,42.7083333469893,23.));
#9336=CARTESIAN_POINT('Ctrl Pts',(33.6743371481684,42.5000000136559,33.6743371481683));
#9337=CARTESIAN_POINT('Ctrl Pts',(23.,42.2916666803226,39.8371685740842));
#9338=CARTESIAN_POINT('Ctrl Pts',(12.3256628518317,42.0833333469893,46.));
#9339=CARTESIAN_POINT('Ctrl Pts',(8.45006291411674E-15,41.8750000136559,
46.));
#9340=CARTESIAN_POINT('Ctrl Pts',(-12.3256628518316,41.6666666803226,46.));
#9341=CARTESIAN_POINT('Ctrl Pts',(-23.,41.4583333469893,39.8371685740842));
#9342=CARTESIAN_POINT('Ctrl Pts',(-33.6743371481683,41.2500000136559,33.6743371481684));
#9343=CARTESIAN_POINT('Ctrl Pts',(-39.8371685740842,41.0416666803226,23.));
#9344=CARTESIAN_POINT('Ctrl Pts',(-46.,40.8333333469893,12.3256628518317));
#9345=CARTESIAN_POINT('Ctrl Pts',(-46.,40.6250000136559,0.));
#9346=CARTESIAN_POINT('Ctrl Pts',(-46.,40.4166666803226,-12.3256628518316));
#9347=CARTESIAN_POINT('Ctrl Pts',(-39.8371685740842,40.2083333469893,-23.));
#9348=CARTESIAN_POINT('Ctrl Pts',(-33.6743371481684,40.0000000136559,-33.6743371481684));
#9349=CARTESIAN_POINT('Ctrl Pts',(-23.,39.7916666803226,-39.8371685740842));
#9350=CARTESIAN_POINT('Ctrl Pts',(-12.3256628518317,39.5833333469893,-46.));
#9351=CARTESIAN_POINT('Ctrl Pts',(-2.81668763803891E-15,39.3750000136559,
-46.));
#9352=CARTESIAN_POINT('Ctrl Pts',(12.3256628518316,39.1666666803226,-46.));
#9353=CARTESIAN_POINT('Ctrl Pts',(23.,38.9583333469893,-39.8371685740842));
#9354=CARTESIAN_POINT('Ctrl Pts',(33.6743371481683,38.7500000136559,-33.6743371481684));
#9355=CARTESIAN_POINT('Ctrl Pts',(39.8371685740842,38.5416666803226,-23.));
#9356=CARTESIAN_POINT('Ctrl Pts',(46.,38.3333333469893,-12.3256628518317));
#9357=CARTESIAN_POINT('Ctrl Pts',(46.,38.1250000136559,-5.63337527607782E-15));
#9358=CARTESIAN_POINT('Ctrl Pts',(46.,37.9166666803226,12.3256628518316));
#9359=CARTESIAN_POINT('Ctrl Pts',(39.8371685740842,37.7083333469893,23.));
#9360=CARTESIAN_POINT('Ctrl Pts',(33.6743371481684,37.5000000136559,33.6743371481683));
#9361=CARTESIAN_POINT('Ctrl Pts',(23.,37.2916666803226,39.8371685740842));
#9362=CARTESIAN_POINT('Ctrl Pts',(12.3256628518317,37.0833333469893,46.));
#9363=CARTESIAN_POINT('Ctrl Pts',(8.45006291411674E-15,36.8750000136559,
46.));
#9364=CARTESIAN_POINT('Ctrl Pts',(-12.3256628518316,36.6666666803226,46.));
#9365=CARTESIAN_POINT('Ctrl Pts',(-23.,36.4583333469893,39.8371685740842));
#9366=CARTESIAN_POINT('Ctrl Pts',(-33.6743371481683,36.2500000136559,33.6743371481684));
#9367=CARTESIAN_POINT('Ctrl Pts',(-39.8371685740842,36.0416666803226,23.));
#9368=CARTESIAN_POINT('Ctrl Pts',(-46.,35.8333333469893,12.3256628518317));
#9369=CARTESIAN_POINT('Ctrl Pts',(-46.,35.6250000136559,0.));
#9370=CARTESIAN_POINT('Ctrl Pts',(-46.,35.4166666803226,-12.3256628518316));
#9371=CARTESIAN_POINT('Ctrl Pts',(-39.8371685740842,35.2083333469893,-23.));
#9372=CARTESIAN_POINT('Ctrl Pts',(-33.6743371481684,35.0000000136559,-33.6743371481684));
#9373=CARTESIAN_POINT('Ctrl Pts',(-23.,34.7916666803226,-39.8371685740842));
#9374=CARTESIAN_POINT('Ctrl Pts',(-12.3256628518317,34.5833333469893,-46.));
#9375=CARTESIAN_POINT('Ctrl Pts',(-2.81668763803891E-15,34.3750000136559,
-46.));
#9376=CARTESIAN_POINT('Ctrl Pts',(12.3256628518316,34.1666666803226,-46.));
#9377=CARTESIAN_POINT('Ctrl Pts',(23.,33.9583333469893,-39.8371685740842));
#9378=CARTESIAN_POINT('Ctrl Pts',(33.6743371481683,33.7500000136559,-33.6743371481684));
#9379=CARTESIAN_POINT('Ctrl Pts',(39.8371685740842,33.5416666803226,-23.));
#9380=CARTESIAN_POINT('Ctrl Pts',(46.,33.3333333469893,-12.3256628518317));
#9381=CARTESIAN_POINT('Ctrl Pts',(46.,33.1250000136559,-5.63337527607782E-15));
#9382=CARTESIAN_POINT('Ctrl Pts',(46.,32.9166666803226,12.3256628518316));
#9383=CARTESIAN_POINT('Ctrl Pts',(39.8371685740842,32.7083333469893,23.));
#9384=CARTESIAN_POINT('Ctrl Pts',(33.6743371481684,32.5000000136559,33.6743371481683));
#9385=CARTESIAN_POINT('Ctrl Pts',(23.,32.2916666803226,39.8371685740842));
#9386=CARTESIAN_POINT('Ctrl Pts',(12.3256628518317,32.0833333469893,46.));
#9387=CARTESIAN_POINT('Ctrl Pts',(8.45006291411674E-15,31.8750000136559,
46.));
#9388=CARTESIAN_POINT('Ctrl Pts',(-12.3256628518316,31.6666666803226,46.));
#9389=CARTESIAN_POINT('Ctrl Pts',(-23.,31.4583333469893,39.8371685740842));
#9390=CARTESIAN_POINT('Ctrl Pts',(-33.6743371481683,31.2500000136559,33.6743371481684));
#9391=CARTESIAN_POINT('Ctrl Pts',(-39.8371685740842,31.0416666803226,23.));
#9392=CARTESIAN_POINT('Ctrl Pts',(-46.,30.8333333469893,12.3256628518317));
#9393=CARTESIAN_POINT('Ctrl Pts',(-46.,30.6250000136559,0.));
#9394=CARTESIAN_POINT('Ctrl Pts',(-46.,30.4166666803226,-12.3256628518316));
#9395=CARTESIAN_POINT('Ctrl Pts',(-39.8371685740842,30.2083333469893,-23.));
#9396=CARTESIAN_POINT('Ctrl Pts',(-33.6743371481684,30.0000000136559,-33.6743371481684));
#9397=CARTESIAN_POINT('Ctrl Pts',(-23.,29.7916666803226,-39.8371685740842));
#9398=CARTESIAN_POINT('Ctrl Pts',(-12.3256628518317,29.5833333469893,-46.));
#9399=CARTESIAN_POINT('Ctrl Pts',(-2.81668763803891E-15,29.3750000136559,
-46.));
#9400=CARTESIAN_POINT('Ctrl Pts',(12.3256628518316,29.1666666803226,-46.));
#9401=CARTESIAN_POINT('Ctrl Pts',(23.,28.9583333469893,-39.8371685740842));
#9402=CARTESIAN_POINT('Ctrl Pts',(33.6743371481683,28.7500000136559,-33.6743371481684));
#9403=CARTESIAN_POINT('Ctrl Pts',(39.8371685740842,28.5416666803226,-23.));
#9404=CARTESIAN_POINT('Ctrl Pts',(46.,28.3333333469893,-12.3256628518317));
#9405=CARTESIAN_POINT('Ctrl Pts',(46.,28.1250000136559,-5.63337527607782E-15));
#9406=CARTESIAN_POINT('Ctrl Pts',(46.,27.9166666803226,12.3256628518316));
#9407=CARTESIAN_POINT('Ctrl Pts',(39.8371685740842,27.7083333469893,23.));
#9408=CARTESIAN_POINT('Ctrl Pts',(33.6743371481684,27.5000000136559,33.6743371481683));
#9409=CARTESIAN_POINT('Ctrl Pts',(23.,27.2916666803226,39.8371685740842));
#9410=CARTESIAN_POINT('Ctrl Pts',(12.3256628518317,27.0833333469893,46.));
#9411=CARTESIAN_POINT('Ctrl Pts',(8.45006291411674E-15,26.8750000136559,
46.));
#9412=CARTESIAN_POINT('Ctrl Pts',(-12.3256628518316,26.6666666803226,46.));
#9413=CARTESIAN_POINT('Ctrl Pts',(-23.,26.4583333469893,39.8371685740842));
#9414=CARTESIAN_POINT('Ctrl Pts',(-33.6743371481683,26.2500000136559,33.6743371481684));
#9415=CARTESIAN_POINT('Ctrl Pts',(-39.8371685740842,26.0416666803226,23.));
#9416=CARTESIAN_POINT('Ctrl Pts',(-46.,25.8333333469893,12.3256628518317));
#9417=CARTESIAN_POINT('Ctrl Pts',(-46.,25.6250000136559,0.));
#9418=CARTESIAN_POINT('Ctrl Pts',(-48.706329375,57.187500006828,-1.8898197019151E-14));
#9419=CARTESIAN_POINT('Ctrl Pts',(-48.706329375,56.9791666734946,-13.0508216223155));
#9420=CARTESIAN_POINT('Ctrl Pts',(-42.1809185638422,56.7708333401613,-24.3531646875));
#9421=CARTESIAN_POINT('Ctrl Pts',(-35.6555077526845,56.562500006828,-35.6555077526845));
#9422=CARTESIAN_POINT('Ctrl Pts',(-24.3531646875,56.3541666734946,-42.1809185638423));
#9423=CARTESIAN_POINT('Ctrl Pts',(-13.0508216223155,56.1458333401613,-48.706329375));
#9424=CARTESIAN_POINT('Ctrl Pts',(1.59157945007855E-14,55.937500006828,
-48.706329375));
#9425=CARTESIAN_POINT('Ctrl Pts',(13.0508216223155,55.7291666734946,-48.706329375));
#9426=CARTESIAN_POINT('Ctrl Pts',(24.3531646875,55.5208333401613,-42.1809185638422));
#9427=CARTESIAN_POINT('Ctrl Pts',(35.6555077526845,55.312500006828,-35.6555077526845));
#9428=CARTESIAN_POINT('Ctrl Pts',(42.1809185638422,55.1041666734946,-24.3531646875));
#9429=CARTESIAN_POINT('Ctrl Pts',(48.706329375,54.8958333401613,-13.0508216223155));
#9430=CARTESIAN_POINT('Ctrl Pts',(48.706329375,54.687500006828,1.293339198242E-14));
#9431=CARTESIAN_POINT('Ctrl Pts',(48.706329375,54.4791666734946,13.0508216223155));
#9432=CARTESIAN_POINT('Ctrl Pts',(42.1809185638422,54.2708333401613,24.3531646875));
#9433=CARTESIAN_POINT('Ctrl Pts',(35.6555077526845,54.062500006828,35.6555077526845));
#9434=CARTESIAN_POINT('Ctrl Pts',(24.3531646875,53.8541666734946,42.1809185638422));
#9435=CARTESIAN_POINT('Ctrl Pts',(13.0508216223155,53.6458333401613,48.706329375));
#9436=CARTESIAN_POINT('Ctrl Pts',(-9.95098946405443E-15,53.437500006828,
48.706329375));
#9437=CARTESIAN_POINT('Ctrl Pts',(-13.0508216223155,53.2291666734946,48.706329375));
#9438=CARTESIAN_POINT('Ctrl Pts',(-24.3531646875,53.0208333401613,42.1809185638423));
#9439=CARTESIAN_POINT('Ctrl Pts',(-35.6555077526845,52.812500006828,35.6555077526845));
#9440=CARTESIAN_POINT('Ctrl Pts',(-42.1809185638422,52.6041666734946,24.3531646875));
#9441=CARTESIAN_POINT('Ctrl Pts',(-48.706329375,52.3958333401613,13.0508216223155));
#9442=CARTESIAN_POINT('Ctrl Pts',(-48.706329375,52.187500006828,-1.8898197019151E-14));
#9443=CARTESIAN_POINT('Ctrl Pts',(-48.706329375,51.9791666734946,-13.0508216223155));
#9444=CARTESIAN_POINT('Ctrl Pts',(-42.1809185638422,51.7708333401613,-24.3531646875));
#9445=CARTESIAN_POINT('Ctrl Pts',(-35.6555077526845,51.562500006828,-35.6555077526845));
#9446=CARTESIAN_POINT('Ctrl Pts',(-24.3531646875,51.3541666734946,-42.1809185638423));
#9447=CARTESIAN_POINT('Ctrl Pts',(-13.0508216223155,51.1458333401613,-48.706329375));
#9448=CARTESIAN_POINT('Ctrl Pts',(1.59157945007855E-14,50.937500006828,
-48.706329375));
#9449=CARTESIAN_POINT('Ctrl Pts',(13.0508216223155,50.7291666734946,-48.706329375));
#9450=CARTESIAN_POINT('Ctrl Pts',(24.3531646875,50.5208333401613,-42.1809185638422));
#9451=CARTESIAN_POINT('Ctrl Pts',(35.6555077526845,50.312500006828,-35.6555077526845));
#9452=CARTESIAN_POINT('Ctrl Pts',(42.1809185638422,50.1041666734946,-24.3531646875));
#9453=CARTESIAN_POINT('Ctrl Pts',(48.706329375,49.8958333401613,-13.0508216223155));
#9454=CARTESIAN_POINT('Ctrl Pts',(48.706329375,49.687500006828,1.293339198242E-14));
#9455=CARTESIAN_POINT('Ctrl Pts',(48.706329375,49.4791666734946,13.0508216223155));
#9456=CARTESIAN_POINT('Ctrl Pts',(42.1809185638422,49.2708333401613,24.3531646875));
#9457=CARTESIAN_POINT('Ctrl Pts',(35.6555077526845,49.062500006828,35.6555077526845));
#9458=CARTESIAN_POINT('Ctrl Pts',(24.3531646875,48.8541666734946,42.1809185638422));
#9459=CARTESIAN_POINT('Ctrl Pts',(13.0508216223155,48.6458333401613,48.706329375));
#9460=CARTESIAN_POINT('Ctrl Pts',(-9.95098946405443E-15,48.437500006828,
48.706329375));
#9461=CARTESIAN_POINT('Ctrl Pts',(-13.0508216223155,48.2291666734946,48.706329375));
#9462=CARTESIAN_POINT('Ctrl Pts',(-24.3531646875,48.0208333401613,42.1809185638423));
#9463=CARTESIAN_POINT('Ctrl Pts',(-35.6555077526845,47.812500006828,35.6555077526845));
#9464=CARTESIAN_POINT('Ctrl Pts',(-42.1809185638422,47.6041666734946,24.3531646875));
#9465=CARTESIAN_POINT('Ctrl Pts',(-48.706329375,47.3958333401613,13.0508216223155));
#9466=CARTESIAN_POINT('Ctrl Pts',(-48.706329375,47.187500006828,-1.8898197019151E-14));
#9467=CARTESIAN_POINT('Ctrl Pts',(-48.706329375,46.9791666734946,-13.0508216223155));
#9468=CARTESIAN_POINT('Ctrl Pts',(-42.1809185638422,46.7708333401613,-24.3531646875));
#9469=CARTESIAN_POINT('Ctrl Pts',(-35.6555077526845,46.562500006828,-35.6555077526845));
#9470=CARTESIAN_POINT('Ctrl Pts',(-24.3531646875,46.3541666734946,-42.1809185638423));
#9471=CARTESIAN_POINT('Ctrl Pts',(-13.0508216223155,46.1458333401613,-48.706329375));
#9472=CARTESIAN_POINT('Ctrl Pts',(1.59157945007855E-14,45.937500006828,
-48.706329375));
#9473=CARTESIAN_POINT('Ctrl Pts',(13.0508216223155,45.7291666734946,-48.706329375));
#9474=CARTESIAN_POINT('Ctrl Pts',(24.3531646875,45.5208333401613,-42.1809185638422));
#9475=CARTESIAN_POINT('Ctrl Pts',(35.6555077526845,45.312500006828,-35.6555077526845));
#9476=CARTESIAN_POINT('Ctrl Pts',(42.1809185638422,45.1041666734946,-24.3531646875));
#9477=CARTESIAN_POINT('Ctrl Pts',(48.706329375,44.8958333401613,-13.0508216223155));
#9478=CARTESIAN_POINT('Ctrl Pts',(48.706329375,44.687500006828,1.293339198242E-14));
#9479=CARTESIAN_POINT('Ctrl Pts',(48.706329375,44.4791666734946,13.0508216223155));
#9480=CARTESIAN_POINT('Ctrl Pts',(42.1809185638422,44.2708333401613,24.3531646875));
#9481=CARTESIAN_POINT('Ctrl Pts',(35.6555077526845,44.062500006828,35.6555077526845));
#9482=CARTESIAN_POINT('Ctrl Pts',(24.3531646875,43.8541666734946,42.1809185638422));
#9483=CARTESIAN_POINT('Ctrl Pts',(13.0508216223155,43.6458333401613,48.706329375));
#9484=CARTESIAN_POINT('Ctrl Pts',(-9.95098946405443E-15,43.437500006828,
48.706329375));
#9485=CARTESIAN_POINT('Ctrl Pts',(-13.0508216223155,43.2291666734946,48.706329375));
#9486=CARTESIAN_POINT('Ctrl Pts',(-24.3531646875,43.0208333401613,42.1809185638423));
#9487=CARTESIAN_POINT('Ctrl Pts',(-35.6555077526845,42.812500006828,35.6555077526845));
#9488=CARTESIAN_POINT('Ctrl Pts',(-42.1809185638422,42.6041666734946,24.3531646875));
#9489=CARTESIAN_POINT('Ctrl Pts',(-48.706329375,42.3958333401613,13.0508216223155));
#9490=CARTESIAN_POINT('Ctrl Pts',(-48.706329375,42.187500006828,-1.8898197019151E-14));
#9491=CARTESIAN_POINT('Ctrl Pts',(-48.706329375,41.9791666734946,-13.0508216223155));
#9492=CARTESIAN_POINT('Ctrl Pts',(-42.1809185638422,41.7708333401613,-24.3531646875));
#9493=CARTESIAN_POINT('Ctrl Pts',(-35.6555077526845,41.562500006828,-35.6555077526845));
#9494=CARTESIAN_POINT('Ctrl Pts',(-24.3531646875,41.3541666734946,-42.1809185638423));
#9495=CARTESIAN_POINT('Ctrl Pts',(-13.0508216223155,41.1458333401613,-48.706329375));
#9496=CARTESIAN_POINT('Ctrl Pts',(1.59157945007855E-14,40.937500006828,
-48.706329375));
#9497=CARTESIAN_POINT('Ctrl Pts',(13.0508216223155,40.7291666734946,-48.706329375));
#9498=CARTESIAN_POINT('Ctrl Pts',(24.3531646875,40.5208333401613,-42.1809185638422));
#9499=CARTESIAN_POINT('Ctrl Pts',(35.6555077526845,40.312500006828,-35.6555077526845));
#9500=CARTESIAN_POINT('Ctrl Pts',(42.1809185638422,40.1041666734946,-24.3531646875));
#9501=CARTESIAN_POINT('Ctrl Pts',(48.706329375,39.8958333401613,-13.0508216223155));
#9502=CARTESIAN_POINT('Ctrl Pts',(48.706329375,39.687500006828,1.293339198242E-14));
#9503=CARTESIAN_POINT('Ctrl Pts',(48.706329375,39.4791666734946,13.0508216223155));
#9504=CARTESIAN_POINT('Ctrl Pts',(42.1809185638422,39.2708333401613,24.3531646875));
#9505=CARTESIAN_POINT('Ctrl Pts',(35.6555077526845,39.062500006828,35.6555077526845));
#9506=CARTESIAN_POINT('Ctrl Pts',(24.3531646875,38.8541666734946,42.1809185638422));
#9507=CARTESIAN_POINT('Ctrl Pts',(13.0508216223155,38.6458333401613,48.706329375));
#9508=CARTESIAN_POINT('Ctrl Pts',(-9.95098946405443E-15,38.437500006828,
48.706329375));
#9509=CARTESIAN_POINT('Ctrl Pts',(-13.0508216223155,38.2291666734946,48.706329375));
#9510=CARTESIAN_POINT('Ctrl Pts',(-24.3531646875,38.0208333401613,42.1809185638423));
#9511=CARTESIAN_POINT('Ctrl Pts',(-35.6555077526845,37.812500006828,35.6555077526845));
#9512=CARTESIAN_POINT('Ctrl Pts',(-42.1809185638422,37.6041666734946,24.3531646875));
#9513=CARTESIAN_POINT('Ctrl Pts',(-48.706329375,37.3958333401613,13.0508216223155));
#9514=CARTESIAN_POINT('Ctrl Pts',(-48.706329375,37.187500006828,-1.8898197019151E-14));
#9515=CARTESIAN_POINT('Ctrl Pts',(-48.706329375,36.9791666734946,-13.0508216223155));
#9516=CARTESIAN_POINT('Ctrl Pts',(-42.1809185638422,36.7708333401613,-24.3531646875));
#9517=CARTESIAN_POINT('Ctrl Pts',(-35.6555077526845,36.562500006828,-35.6555077526845));
#9518=CARTESIAN_POINT('Ctrl Pts',(-24.3531646875,36.3541666734946,-42.1809185638423));
#9519=CARTESIAN_POINT('Ctrl Pts',(-13.0508216223155,36.1458333401613,-48.706329375));
#9520=CARTESIAN_POINT('Ctrl Pts',(1.59157945007855E-14,35.937500006828,
-48.706329375));
#9521=CARTESIAN_POINT('Ctrl Pts',(13.0508216223155,35.7291666734946,-48.706329375));
#9522=CARTESIAN_POINT('Ctrl Pts',(24.3531646875,35.5208333401613,-42.1809185638422));
#9523=CARTESIAN_POINT('Ctrl Pts',(35.6555077526845,35.312500006828,-35.6555077526845));
#9524=CARTESIAN_POINT('Ctrl Pts',(42.1809185638422,35.1041666734946,-24.3531646875));
#9525=CARTESIAN_POINT('Ctrl Pts',(48.706329375,34.8958333401613,-13.0508216223155));
#9526=CARTESIAN_POINT('Ctrl Pts',(48.706329375,34.687500006828,1.293339198242E-14));
#9527=CARTESIAN_POINT('Ctrl Pts',(48.706329375,34.4791666734946,13.0508216223155));
#9528=CARTESIAN_POINT('Ctrl Pts',(42.1809185638422,34.2708333401613,24.3531646875));
#9529=CARTESIAN_POINT('Ctrl Pts',(35.6555077526845,34.062500006828,35.6555077526845));
#9530=CARTESIAN_POINT('Ctrl Pts',(24.3531646875,33.8541666734946,42.1809185638422));
#9531=CARTESIAN_POINT('Ctrl Pts',(13.0508216223155,33.6458333401613,48.706329375));
#9532=CARTESIAN_POINT('Ctrl Pts',(-9.95098946405443E-15,33.437500006828,
48.706329375));
#9533=CARTESIAN_POINT('Ctrl Pts',(-13.0508216223155,33.2291666734946,48.706329375));
#9534=CARTESIAN_POINT('Ctrl Pts',(-24.3531646875,33.0208333401613,42.1809185638423));
#9535=CARTESIAN_POINT('Ctrl Pts',(-35.6555077526845,32.812500006828,35.6555077526845));
#9536=CARTESIAN_POINT('Ctrl Pts',(-42.1809185638422,32.6041666734946,24.3531646875));
#9537=CARTESIAN_POINT('Ctrl Pts',(-48.706329375,32.3958333401613,13.0508216223155));
#9538=CARTESIAN_POINT('Ctrl Pts',(-48.706329375,32.187500006828,-1.8898197019151E-14));
#9539=CARTESIAN_POINT('Ctrl Pts',(-48.706329375,31.9791666734946,-13.0508216223155));
#9540=CARTESIAN_POINT('Ctrl Pts',(-42.1809185638422,31.7708333401613,-24.3531646875));
#9541=CARTESIAN_POINT('Ctrl Pts',(-35.6555077526845,31.562500006828,-35.6555077526845));
#9542=CARTESIAN_POINT('Ctrl Pts',(-24.3531646875,31.3541666734946,-42.1809185638423));
#9543=CARTESIAN_POINT('Ctrl Pts',(-13.0508216223155,31.1458333401613,-48.706329375));
#9544=CARTESIAN_POINT('Ctrl Pts',(1.59157945007855E-14,30.937500006828,
-48.706329375));
#9545=CARTESIAN_POINT('Ctrl Pts',(13.0508216223155,30.7291666734946,-48.706329375));
#9546=CARTESIAN_POINT('Ctrl Pts',(24.3531646875,30.5208333401613,-42.1809185638422));
#9547=CARTESIAN_POINT('Ctrl Pts',(35.6555077526845,30.312500006828,-35.6555077526845));
#9548=CARTESIAN_POINT('Ctrl Pts',(42.1809185638422,30.1041666734946,-24.3531646875));
#9549=CARTESIAN_POINT('Ctrl Pts',(48.706329375,29.8958333401613,-13.0508216223155));
#9550=CARTESIAN_POINT('Ctrl Pts',(48.706329375,29.687500006828,1.293339198242E-14));
#9551=CARTESIAN_POINT('Ctrl Pts',(48.706329375,29.4791666734946,13.0508216223155));
#9552=CARTESIAN_POINT('Ctrl Pts',(42.1809185638422,29.2708333401613,24.3531646875));
#9553=CARTESIAN_POINT('Ctrl Pts',(35.6555077526845,29.062500006828,35.6555077526845));
#9554=CARTESIAN_POINT('Ctrl Pts',(24.3531646875,28.8541666734946,42.1809185638422));
#9555=CARTESIAN_POINT('Ctrl Pts',(13.0508216223155,28.6458333401613,48.706329375));
#9556=CARTESIAN_POINT('Ctrl Pts',(-9.95098946405443E-15,28.437500006828,
48.706329375));
#9557=CARTESIAN_POINT('Ctrl Pts',(-13.0508216223155,28.2291666734946,48.706329375));
#9558=CARTESIAN_POINT('Ctrl Pts',(-24.3531646875,28.0208333401613,42.1809185638423));
#9559=CARTESIAN_POINT('Ctrl Pts',(-35.6555077526845,27.812500006828,35.6555077526845));
#9560=CARTESIAN_POINT('Ctrl Pts',(-42.1809185638422,27.6041666734946,24.3531646875));
#9561=CARTESIAN_POINT('Ctrl Pts',(-48.706329375,27.3958333401613,13.0508216223155));
#9562=CARTESIAN_POINT('Ctrl Pts',(-48.706329375,27.187500006828,-1.8898197019151E-14));
#9563=CARTESIAN_POINT('',(-4.32456003949883,48.3676432269777,48.5139639861634));
#9564=CARTESIAN_POINT('',(-48.5725845633798,47.2456516907297,3.60701400320326));
#9565=CARTESIAN_POINT('Ctrl Pts',(-4.32456003949883,48.3676432269777,48.5139639861634));
#9566=CARTESIAN_POINT('Ctrl Pts',(-15.0381414154991,48.1925348924095,47.5589497574396));
#9567=CARTESIAN_POINT('Ctrl Pts',(-24.3531646875,48.0208333401613,42.1809185638423));
#9568=CARTESIAN_POINT('Ctrl Pts',(-35.6555077526845,47.812500006828,35.6555077526845));
#9569=CARTESIAN_POINT('Ctrl Pts',(-42.1809185638422,47.6041666734946,24.3531646875));
#9570=CARTESIAN_POINT('Ctrl Pts',(-47.7480251419552,47.4264286116308,14.7106532430575));
#9571=CARTESIAN_POINT('Ctrl Pts',(-48.5725845633798,47.2456516907297,3.60701400320326));
#9572=CARTESIAN_POINT('Ctrl Pts',(-48.5725845633798,47.2456516907297,3.60701400320326));
#9573=CARTESIAN_POINT('Ctrl Pts',(-48.3407853679392,47.1124685639422,3.60701400320326));
#9574=CARTESIAN_POINT('Ctrl Pts',(-48.1089821836664,46.9792923792741,3.60701400320326));
#9575=CARTESIAN_POINT('Ctrl Pts',(-47.6453674864979,46.7129545080418,3.60701400320326));
#9576=CARTESIAN_POINT('Ctrl Pts',(-47.4135559734253,46.5797928212585,3.60701400320325));
#9577=CARTESIAN_POINT('Ctrl Pts',(-47.1817401099609,46.4466387085919,3.60701400320325));
#9578=CARTESIAN_POINT('Ctrl Pts',(-46.7406305897488,46.1932671494809,3.60701400320325));
#9579=CARTESIAN_POINT('Ctrl Pts',(-46.2995053259033,45.9399229970588,3.60701400320326));
#9580=CARTESIAN_POINT('Ctrl Pts',(-45.858362923034,45.686608693912,3.60701400320327));
#9581=CARTESIAN_POINT('Ctrl Pts',(-4.32456003949882,46.8009818542622,45.7962681936506));
#9582=CARTESIAN_POINT('Ctrl Pts',(-4.32456003949882,46.9344874667937,46.0278818021281));
#9583=CARTESIAN_POINT('Ctrl Pts',(-4.32456003949869,47.2015035419424,46.4911062234486));
#9584=CARTESIAN_POINT('Ctrl Pts',(-4.32456003949883,47.4685288945405,46.954325296818));
#9585=CARTESIAN_POINT('Ctrl Pts',(-4.32456003949883,47.8572357107336,47.6286149142205));
#9586=CARTESIAN_POINT('Ctrl Pts',(-4.32456003949883,48.1124357360102,48.0712916022845));
#9587=CARTESIAN_POINT('Ctrl Pts',(-4.32456003949883,48.3676432269777,48.5139639861634));
#9588=CARTESIAN_POINT('Ctrl Pts',(-46.,55.6250000136559,0.));
#9589=CARTESIAN_POINT('Ctrl Pts',(-46.,55.4166666803226,-12.3256628518316));
#9590=CARTESIAN_POINT('Ctrl Pts',(-39.8371685740842,55.2083333469893,-23.));
#9591=CARTESIAN_POINT('Ctrl Pts',(-33.6743371481684,55.0000000136559,-33.6743371481684));
#9592=CARTESIAN_POINT('Ctrl Pts',(-23.,54.7916666803226,-39.8371685740842));
#9593=CARTESIAN_POINT('Ctrl Pts',(-12.3256628518317,54.5833333469893,-46.));
#9594=CARTESIAN_POINT('Ctrl Pts',(-2.81668763803891E-15,54.3750000136559,
-46.));
#9595=CARTESIAN_POINT('Ctrl Pts',(12.3256628518316,54.1666666803226,-46.));
#9596=CARTESIAN_POINT('Ctrl Pts',(23.,53.9583333469893,-39.8371685740842));
#9597=CARTESIAN_POINT('Ctrl Pts',(33.6743371481683,53.7500000136559,-33.6743371481684));
#9598=CARTESIAN_POINT('Ctrl Pts',(39.8371685740842,53.5416666803226,-23.));
#9599=CARTESIAN_POINT('Ctrl Pts',(46.,53.3333333469893,-12.3256628518317));
#9600=CARTESIAN_POINT('Ctrl Pts',(46.,53.1250000136559,-5.63337527607782E-15));
#9601=CARTESIAN_POINT('Ctrl Pts',(46.,52.9166666803226,12.3256628518316));
#9602=CARTESIAN_POINT('Ctrl Pts',(39.8371685740842,52.7083333469893,23.));
#9603=CARTESIAN_POINT('Ctrl Pts',(33.6743371481684,52.5000000136559,33.6743371481683));
#9604=CARTESIAN_POINT('Ctrl Pts',(23.,52.2916666803226,39.8371685740842));
#9605=CARTESIAN_POINT('Ctrl Pts',(12.3256628518317,52.0833333469893,46.));
#9606=CARTESIAN_POINT('Ctrl Pts',(8.45006291411674E-15,51.8750000136559,
46.));
#9607=CARTESIAN_POINT('Ctrl Pts',(-12.3256628518316,51.6666666803226,46.));
#9608=CARTESIAN_POINT('Ctrl Pts',(-23.,51.4583333469893,39.8371685740842));
#9609=CARTESIAN_POINT('Ctrl Pts',(-33.6743371481683,51.2500000136559,33.6743371481684));
#9610=CARTESIAN_POINT('Ctrl Pts',(-39.8371685740842,51.0416666803226,23.));
#9611=CARTESIAN_POINT('Ctrl Pts',(-46.,50.8333333469893,12.3256628518317));
#9612=CARTESIAN_POINT('Ctrl Pts',(-46.,50.6250000136559,0.));
#9613=CARTESIAN_POINT('Ctrl Pts',(-46.,50.4166666803226,-12.3256628518316));
#9614=CARTESIAN_POINT('Ctrl Pts',(-39.8371685740842,50.2083333469893,-23.));
#9615=CARTESIAN_POINT('Ctrl Pts',(-33.6743371481684,50.0000000136559,-33.6743371481684));
#9616=CARTESIAN_POINT('Ctrl Pts',(-23.,49.7916666803226,-39.8371685740842));
#9617=CARTESIAN_POINT('Ctrl Pts',(-12.3256628518317,49.5833333469893,-46.));
#9618=CARTESIAN_POINT('Ctrl Pts',(-2.81668763803891E-15,49.3750000136559,
-46.));
#9619=CARTESIAN_POINT('Ctrl Pts',(12.3256628518316,49.1666666803226,-46.));
#9620=CARTESIAN_POINT('Ctrl Pts',(23.,48.9583333469893,-39.8371685740842));
#9621=CARTESIAN_POINT('Ctrl Pts',(33.6743371481683,48.7500000136559,-33.6743371481684));
#9622=CARTESIAN_POINT('Ctrl Pts',(39.8371685740842,48.5416666803226,-23.));
#9623=CARTESIAN_POINT('Ctrl Pts',(46.,48.3333333469893,-12.3256628518317));
#9624=CARTESIAN_POINT('Ctrl Pts',(46.,48.1250000136559,-5.63337527607782E-15));
#9625=CARTESIAN_POINT('Ctrl Pts',(46.,47.9166666803226,12.3256628518316));
#9626=CARTESIAN_POINT('Ctrl Pts',(39.8371685740842,47.7083333469893,23.));
#9627=CARTESIAN_POINT('Ctrl Pts',(33.6743371481684,47.5000000136559,33.6743371481683));
#9628=CARTESIAN_POINT('Ctrl Pts',(23.,47.2916666803226,39.8371685740842));
#9629=CARTESIAN_POINT('Ctrl Pts',(12.3256628518317,47.0833333469893,46.));
#9630=CARTESIAN_POINT('Ctrl Pts',(8.45006291411674E-15,46.8750000136559,
46.));
#9631=CARTESIAN_POINT('Ctrl Pts',(-12.3256628518316,46.6666666803226,46.));
#9632=CARTESIAN_POINT('Ctrl Pts',(-23.,46.4583333469893,39.8371685740842));
#9633=CARTESIAN_POINT('Ctrl Pts',(-33.6743371481683,46.2500000136559,33.6743371481684));
#9634=CARTESIAN_POINT('Ctrl Pts',(-39.8371685740842,46.0416666803226,23.));
#9635=CARTESIAN_POINT('Ctrl Pts',(-46.,45.8333333469892,12.3256628518317));
#9636=CARTESIAN_POINT('Ctrl Pts',(-46.,45.6250000136559,0.));
#9637=CARTESIAN_POINT('Ctrl Pts',(-46.,45.4166666803226,-12.3256628518316));
#9638=CARTESIAN_POINT('Ctrl Pts',(-39.8371685740842,45.2083333469893,-23.));
#9639=CARTESIAN_POINT('Ctrl Pts',(-33.6743371481684,45.0000000136559,-33.6743371481684));
#9640=CARTESIAN_POINT('Ctrl Pts',(-23.,44.7916666803226,-39.8371685740842));
#9641=CARTESIAN_POINT('Ctrl Pts',(-12.3256628518317,44.5833333469893,-46.));
#9642=CARTESIAN_POINT('Ctrl Pts',(-2.81668763803891E-15,44.3750000136559,
-46.));
#9643=CARTESIAN_POINT('Ctrl Pts',(12.3256628518316,44.1666666803226,-46.));
#9644=CARTESIAN_POINT('Ctrl Pts',(23.,43.9583333469893,-39.8371685740842));
#9645=CARTESIAN_POINT('Ctrl Pts',(33.6743371481683,43.7500000136559,-33.6743371481684));
#9646=CARTESIAN_POINT('Ctrl Pts',(39.8371685740842,43.5416666803226,-23.));
#9647=CARTESIAN_POINT('Ctrl Pts',(46.,43.3333333469893,-12.3256628518317));
#9648=CARTESIAN_POINT('Ctrl Pts',(46.,43.1250000136559,-5.63337527607782E-15));
#9649=CARTESIAN_POINT('Ctrl Pts',(46.,42.9166666803226,12.3256628518316));
#9650=CARTESIAN_POINT('Ctrl Pts',(39.8371685740842,42.7083333469893,23.));
#9651=CARTESIAN_POINT('Ctrl Pts',(33.6743371481684,42.5000000136559,33.6743371481683));
#9652=CARTESIAN_POINT('Ctrl Pts',(23.,42.2916666803226,39.8371685740842));
#9653=CARTESIAN_POINT('Ctrl Pts',(12.3256628518317,42.0833333469893,46.));
#9654=CARTESIAN_POINT('Ctrl Pts',(8.45006291411674E-15,41.8750000136559,
46.));
#9655=CARTESIAN_POINT('Ctrl Pts',(-12.3256628518316,41.6666666803226,46.));
#9656=CARTESIAN_POINT('Ctrl Pts',(-23.,41.4583333469893,39.8371685740842));
#9657=CARTESIAN_POINT('Ctrl Pts',(-33.6743371481683,41.2500000136559,33.6743371481684));
#9658=CARTESIAN_POINT('Ctrl Pts',(-39.8371685740842,41.0416666803226,23.));
#9659=CARTESIAN_POINT('Ctrl Pts',(-46.,40.8333333469893,12.3256628518317));
#9660=CARTESIAN_POINT('Ctrl Pts',(-46.,40.6250000136559,0.));
#9661=CARTESIAN_POINT('Ctrl Pts',(-46.,40.4166666803226,-12.3256628518316));
#9662=CARTESIAN_POINT('Ctrl Pts',(-39.8371685740842,40.2083333469893,-23.));
#9663=CARTESIAN_POINT('Ctrl Pts',(-33.6743371481684,40.0000000136559,-33.6743371481684));
#9664=CARTESIAN_POINT('Ctrl Pts',(-23.,39.7916666803226,-39.8371685740842));
#9665=CARTESIAN_POINT('Ctrl Pts',(-12.3256628518317,39.5833333469893,-46.));
#9666=CARTESIAN_POINT('Ctrl Pts',(-2.81668763803891E-15,39.3750000136559,
-46.));
#9667=CARTESIAN_POINT('Ctrl Pts',(12.3256628518316,39.1666666803226,-46.));
#9668=CARTESIAN_POINT('Ctrl Pts',(23.,38.9583333469893,-39.8371685740842));
#9669=CARTESIAN_POINT('Ctrl Pts',(33.6743371481683,38.7500000136559,-33.6743371481684));
#9670=CARTESIAN_POINT('Ctrl Pts',(39.8371685740842,38.5416666803226,-23.));
#9671=CARTESIAN_POINT('Ctrl Pts',(46.,38.3333333469893,-12.3256628518317));
#9672=CARTESIAN_POINT('Ctrl Pts',(46.,38.1250000136559,-5.63337527607782E-15));
#9673=CARTESIAN_POINT('Ctrl Pts',(46.,37.9166666803226,12.3256628518316));
#9674=CARTESIAN_POINT('Ctrl Pts',(39.8371685740842,37.7083333469893,23.));
#9675=CARTESIAN_POINT('Ctrl Pts',(33.6743371481684,37.5000000136559,33.6743371481683));
#9676=CARTESIAN_POINT('Ctrl Pts',(23.,37.2916666803226,39.8371685740842));
#9677=CARTESIAN_POINT('Ctrl Pts',(12.3256628518317,37.0833333469893,46.));
#9678=CARTESIAN_POINT('Ctrl Pts',(8.45006291411674E-15,36.8750000136559,
46.));
#9679=CARTESIAN_POINT('Ctrl Pts',(-12.3256628518316,36.6666666803226,46.));
#9680=CARTESIAN_POINT('Ctrl Pts',(-23.,36.4583333469893,39.8371685740842));
#9681=CARTESIAN_POINT('Ctrl Pts',(-33.6743371481683,36.2500000136559,33.6743371481684));
#9682=CARTESIAN_POINT('Ctrl Pts',(-39.8371685740842,36.0416666803226,23.));
#9683=CARTESIAN_POINT('Ctrl Pts',(-46.,35.8333333469893,12.3256628518317));
#9684=CARTESIAN_POINT('Ctrl Pts',(-46.,35.6250000136559,0.));
#9685=CARTESIAN_POINT('Ctrl Pts',(-46.,35.4166666803226,-12.3256628518316));
#9686=CARTESIAN_POINT('Ctrl Pts',(-39.8371685740842,35.2083333469893,-23.));
#9687=CARTESIAN_POINT('Ctrl Pts',(-33.6743371481684,35.0000000136559,-33.6743371481684));
#9688=CARTESIAN_POINT('Ctrl Pts',(-23.,34.7916666803226,-39.8371685740842));
#9689=CARTESIAN_POINT('Ctrl Pts',(-12.3256628518317,34.5833333469893,-46.));
#9690=CARTESIAN_POINT('Ctrl Pts',(-2.81668763803891E-15,34.3750000136559,
-46.));
#9691=CARTESIAN_POINT('Ctrl Pts',(12.3256628518316,34.1666666803226,-46.));
#9692=CARTESIAN_POINT('Ctrl Pts',(23.,33.9583333469893,-39.8371685740842));
#9693=CARTESIAN_POINT('Ctrl Pts',(33.6743371481683,33.7500000136559,-33.6743371481684));
#9694=CARTESIAN_POINT('Ctrl Pts',(39.8371685740842,33.5416666803226,-23.));
#9695=CARTESIAN_POINT('Ctrl Pts',(46.,33.3333333469893,-12.3256628518317));
#9696=CARTESIAN_POINT('Ctrl Pts',(46.,33.1250000136559,-5.63337527607782E-15));
#9697=CARTESIAN_POINT('Ctrl Pts',(46.,32.9166666803226,12.3256628518316));
#9698=CARTESIAN_POINT('Ctrl Pts',(39.8371685740842,32.7083333469893,23.));
#9699=CARTESIAN_POINT('Ctrl Pts',(33.6743371481684,32.5000000136559,33.6743371481683));
#9700=CARTESIAN_POINT('Ctrl Pts',(23.,32.2916666803226,39.8371685740842));
#9701=CARTESIAN_POINT('Ctrl Pts',(12.3256628518317,32.0833333469893,46.));
#9702=CARTESIAN_POINT('Ctrl Pts',(8.45006291411674E-15,31.8750000136559,
46.));
#9703=CARTESIAN_POINT('Ctrl Pts',(-12.3256628518316,31.6666666803226,46.));
#9704=CARTESIAN_POINT('Ctrl Pts',(-23.,31.4583333469893,39.8371685740842));
#9705=CARTESIAN_POINT('Ctrl Pts',(-33.6743371481683,31.2500000136559,33.6743371481684));
#9706=CARTESIAN_POINT('Ctrl Pts',(-39.8371685740842,31.0416666803226,23.));
#9707=CARTESIAN_POINT('Ctrl Pts',(-46.,30.8333333469893,12.3256628518317));
#9708=CARTESIAN_POINT('Ctrl Pts',(-46.,30.6250000136559,0.));
#9709=CARTESIAN_POINT('Ctrl Pts',(-46.,30.4166666803226,-12.3256628518316));
#9710=CARTESIAN_POINT('Ctrl Pts',(-39.8371685740842,30.2083333469893,-23.));
#9711=CARTESIAN_POINT('Ctrl Pts',(-33.6743371481684,30.0000000136559,-33.6743371481684));
#9712=CARTESIAN_POINT('Ctrl Pts',(-23.,29.7916666803226,-39.8371685740842));
#9713=CARTESIAN_POINT('Ctrl Pts',(-12.3256628518317,29.5833333469893,-46.));
#9714=CARTESIAN_POINT('Ctrl Pts',(-2.81668763803891E-15,29.3750000136559,
-46.));
#9715=CARTESIAN_POINT('Ctrl Pts',(12.3256628518316,29.1666666803226,-46.));
#9716=CARTESIAN_POINT('Ctrl Pts',(23.,28.9583333469893,-39.8371685740842));
#9717=CARTESIAN_POINT('Ctrl Pts',(33.6743371481683,28.7500000136559,-33.6743371481684));
#9718=CARTESIAN_POINT('Ctrl Pts',(39.8371685740842,28.5416666803226,-23.));
#9719=CARTESIAN_POINT('Ctrl Pts',(46.,28.3333333469893,-12.3256628518317));
#9720=CARTESIAN_POINT('Ctrl Pts',(46.,28.1250000136559,-5.63337527607782E-15));
#9721=CARTESIAN_POINT('Ctrl Pts',(46.,27.9166666803226,12.3256628518316));
#9722=CARTESIAN_POINT('Ctrl Pts',(39.8371685740842,27.7083333469893,23.));
#9723=CARTESIAN_POINT('Ctrl Pts',(33.6743371481684,27.5000000136559,33.6743371481683));
#9724=CARTESIAN_POINT('Ctrl Pts',(23.,27.2916666803226,39.8371685740842));
#9725=CARTESIAN_POINT('Ctrl Pts',(12.3256628518317,27.0833333469893,46.));
#9726=CARTESIAN_POINT('Ctrl Pts',(8.45006291411674E-15,26.8750000136559,
46.));
#9727=CARTESIAN_POINT('Ctrl Pts',(-12.3256628518316,26.6666666803226,46.));
#9728=CARTESIAN_POINT('Ctrl Pts',(-23.,26.4583333469893,39.8371685740842));
#9729=CARTESIAN_POINT('Ctrl Pts',(-33.6743371481683,26.2500000136559,33.6743371481684));
#9730=CARTESIAN_POINT('Ctrl Pts',(-39.8371685740842,26.0416666803226,23.));
#9731=CARTESIAN_POINT('Ctrl Pts',(-46.,25.8333333469893,12.3256628518317));
#9732=CARTESIAN_POINT('Ctrl Pts',(-46.,25.6250000136559,0.));
#9733=CARTESIAN_POINT('Ctrl Pts',(-48.706329375,57.187500006828,-1.8898197019151E-14));
#9734=CARTESIAN_POINT('Ctrl Pts',(-48.706329375,56.9791666734946,-13.0508216223155));
#9735=CARTESIAN_POINT('Ctrl Pts',(-42.1809185638422,56.7708333401613,-24.3531646875));
#9736=CARTESIAN_POINT('Ctrl Pts',(-35.6555077526845,56.562500006828,-35.6555077526845));
#9737=CARTESIAN_POINT('Ctrl Pts',(-24.3531646875,56.3541666734946,-42.1809185638423));
#9738=CARTESIAN_POINT('Ctrl Pts',(-13.0508216223155,56.1458333401613,-48.706329375));
#9739=CARTESIAN_POINT('Ctrl Pts',(1.59157945007855E-14,55.937500006828,
-48.706329375));
#9740=CARTESIAN_POINT('Ctrl Pts',(13.0508216223155,55.7291666734946,-48.706329375));
#9741=CARTESIAN_POINT('Ctrl Pts',(24.3531646875,55.5208333401613,-42.1809185638422));
#9742=CARTESIAN_POINT('Ctrl Pts',(35.6555077526845,55.312500006828,-35.6555077526845));
#9743=CARTESIAN_POINT('Ctrl Pts',(42.1809185638422,55.1041666734946,-24.3531646875));
#9744=CARTESIAN_POINT('Ctrl Pts',(48.706329375,54.8958333401613,-13.0508216223155));
#9745=CARTESIAN_POINT('Ctrl Pts',(48.706329375,54.687500006828,1.293339198242E-14));
#9746=CARTESIAN_POINT('Ctrl Pts',(48.706329375,54.4791666734946,13.0508216223155));
#9747=CARTESIAN_POINT('Ctrl Pts',(42.1809185638422,54.2708333401613,24.3531646875));
#9748=CARTESIAN_POINT('Ctrl Pts',(35.6555077526845,54.062500006828,35.6555077526845));
#9749=CARTESIAN_POINT('Ctrl Pts',(24.3531646875,53.8541666734946,42.1809185638422));
#9750=CARTESIAN_POINT('Ctrl Pts',(13.0508216223155,53.6458333401613,48.706329375));
#9751=CARTESIAN_POINT('Ctrl Pts',(-9.95098946405443E-15,53.437500006828,
48.706329375));
#9752=CARTESIAN_POINT('Ctrl Pts',(-13.0508216223155,53.2291666734946,48.706329375));
#9753=CARTESIAN_POINT('Ctrl Pts',(-24.3531646875,53.0208333401613,42.1809185638423));
#9754=CARTESIAN_POINT('Ctrl Pts',(-35.6555077526845,52.812500006828,35.6555077526845));
#9755=CARTESIAN_POINT('Ctrl Pts',(-42.1809185638422,52.6041666734946,24.3531646875));
#9756=CARTESIAN_POINT('Ctrl Pts',(-48.706329375,52.3958333401613,13.0508216223155));
#9757=CARTESIAN_POINT('Ctrl Pts',(-48.706329375,52.187500006828,-1.8898197019151E-14));
#9758=CARTESIAN_POINT('Ctrl Pts',(-48.706329375,51.9791666734946,-13.0508216223155));
#9759=CARTESIAN_POINT('Ctrl Pts',(-42.1809185638422,51.7708333401613,-24.3531646875));
#9760=CARTESIAN_POINT('Ctrl Pts',(-35.6555077526845,51.562500006828,-35.6555077526845));
#9761=CARTESIAN_POINT('Ctrl Pts',(-24.3531646875,51.3541666734946,-42.1809185638423));
#9762=CARTESIAN_POINT('Ctrl Pts',(-13.0508216223155,51.1458333401613,-48.706329375));
#9763=CARTESIAN_POINT('Ctrl Pts',(1.59157945007855E-14,50.937500006828,
-48.706329375));
#9764=CARTESIAN_POINT('Ctrl Pts',(13.0508216223155,50.7291666734946,-48.706329375));
#9765=CARTESIAN_POINT('Ctrl Pts',(24.3531646875,50.5208333401613,-42.1809185638422));
#9766=CARTESIAN_POINT('Ctrl Pts',(35.6555077526845,50.312500006828,-35.6555077526845));
#9767=CARTESIAN_POINT('Ctrl Pts',(42.1809185638422,50.1041666734946,-24.3531646875));
#9768=CARTESIAN_POINT('Ctrl Pts',(48.706329375,49.8958333401613,-13.0508216223155));
#9769=CARTESIAN_POINT('Ctrl Pts',(48.706329375,49.687500006828,1.293339198242E-14));
#9770=CARTESIAN_POINT('Ctrl Pts',(48.706329375,49.4791666734946,13.0508216223155));
#9771=CARTESIAN_POINT('Ctrl Pts',(42.1809185638422,49.2708333401613,24.3531646875));
#9772=CARTESIAN_POINT('Ctrl Pts',(35.6555077526845,49.062500006828,35.6555077526845));
#9773=CARTESIAN_POINT('Ctrl Pts',(24.3531646875,48.8541666734946,42.1809185638422));
#9774=CARTESIAN_POINT('Ctrl Pts',(13.0508216223155,48.6458333401613,48.706329375));
#9775=CARTESIAN_POINT('Ctrl Pts',(-9.95098946405443E-15,48.437500006828,
48.706329375));
#9776=CARTESIAN_POINT('Ctrl Pts',(-13.0508216223155,48.2291666734946,48.706329375));
#9777=CARTESIAN_POINT('Ctrl Pts',(-24.3531646875,48.0208333401613,42.1809185638423));
#9778=CARTESIAN_POINT('Ctrl Pts',(-35.6555077526845,47.812500006828,35.6555077526845));
#9779=CARTESIAN_POINT('Ctrl Pts',(-42.1809185638422,47.6041666734946,24.3531646875));
#9780=CARTESIAN_POINT('Ctrl Pts',(-48.706329375,47.3958333401613,13.0508216223155));
#9781=CARTESIAN_POINT('Ctrl Pts',(-48.706329375,47.187500006828,-1.8898197019151E-14));
#9782=CARTESIAN_POINT('Ctrl Pts',(-48.706329375,46.9791666734946,-13.0508216223155));
#9783=CARTESIAN_POINT('Ctrl Pts',(-42.1809185638422,46.7708333401613,-24.3531646875));
#9784=CARTESIAN_POINT('Ctrl Pts',(-35.6555077526845,46.562500006828,-35.6555077526845));
#9785=CARTESIAN_POINT('Ctrl Pts',(-24.3531646875,46.3541666734946,-42.1809185638423));
#9786=CARTESIAN_POINT('Ctrl Pts',(-13.0508216223155,46.1458333401613,-48.706329375));
#9787=CARTESIAN_POINT('Ctrl Pts',(1.59157945007855E-14,45.937500006828,
-48.706329375));
#9788=CARTESIAN_POINT('Ctrl Pts',(13.0508216223155,45.7291666734946,-48.706329375));
#9789=CARTESIAN_POINT('Ctrl Pts',(24.3531646875,45.5208333401613,-42.1809185638422));
#9790=CARTESIAN_POINT('Ctrl Pts',(35.6555077526845,45.312500006828,-35.6555077526845));
#9791=CARTESIAN_POINT('Ctrl Pts',(42.1809185638422,45.1041666734946,-24.3531646875));
#9792=CARTESIAN_POINT('Ctrl Pts',(48.706329375,44.8958333401613,-13.0508216223155));
#9793=CARTESIAN_POINT('Ctrl Pts',(48.706329375,44.687500006828,1.293339198242E-14));
#9794=CARTESIAN_POINT('Ctrl Pts',(48.706329375,44.4791666734946,13.0508216223155));
#9795=CARTESIAN_POINT('Ctrl Pts',(42.1809185638422,44.2708333401613,24.3531646875));
#9796=CARTESIAN_POINT('Ctrl Pts',(35.6555077526845,44.062500006828,35.6555077526845));
#9797=CARTESIAN_POINT('Ctrl Pts',(24.3531646875,43.8541666734946,42.1809185638422));
#9798=CARTESIAN_POINT('Ctrl Pts',(13.0508216223155,43.6458333401613,48.706329375));
#9799=CARTESIAN_POINT('Ctrl Pts',(-9.95098946405443E-15,43.437500006828,
48.706329375));
#9800=CARTESIAN_POINT('Ctrl Pts',(-13.0508216223155,43.2291666734946,48.706329375));
#9801=CARTESIAN_POINT('Ctrl Pts',(-24.3531646875,43.0208333401613,42.1809185638423));
#9802=CARTESIAN_POINT('Ctrl Pts',(-35.6555077526845,42.812500006828,35.6555077526845));
#9803=CARTESIAN_POINT('Ctrl Pts',(-42.1809185638422,42.6041666734946,24.3531646875));
#9804=CARTESIAN_POINT('Ctrl Pts',(-48.706329375,42.3958333401613,13.0508216223155));
#9805=CARTESIAN_POINT('Ctrl Pts',(-48.706329375,42.187500006828,-1.8898197019151E-14));
#9806=CARTESIAN_POINT('Ctrl Pts',(-48.706329375,41.9791666734946,-13.0508216223155));
#9807=CARTESIAN_POINT('Ctrl Pts',(-42.1809185638422,41.7708333401613,-24.3531646875));
#9808=CARTESIAN_POINT('Ctrl Pts',(-35.6555077526845,41.562500006828,-35.6555077526845));
#9809=CARTESIAN_POINT('Ctrl Pts',(-24.3531646875,41.3541666734946,-42.1809185638423));
#9810=CARTESIAN_POINT('Ctrl Pts',(-13.0508216223155,41.1458333401613,-48.706329375));
#9811=CARTESIAN_POINT('Ctrl Pts',(1.59157945007855E-14,40.937500006828,
-48.706329375));
#9812=CARTESIAN_POINT('Ctrl Pts',(13.0508216223155,40.7291666734946,-48.706329375));
#9813=CARTESIAN_POINT('Ctrl Pts',(24.3531646875,40.5208333401613,-42.1809185638422));
#9814=CARTESIAN_POINT('Ctrl Pts',(35.6555077526845,40.312500006828,-35.6555077526845));
#9815=CARTESIAN_POINT('Ctrl Pts',(42.1809185638422,40.1041666734946,-24.3531646875));
#9816=CARTESIAN_POINT('Ctrl Pts',(48.706329375,39.8958333401613,-13.0508216223155));
#9817=CARTESIAN_POINT('Ctrl Pts',(48.706329375,39.687500006828,1.293339198242E-14));
#9818=CARTESIAN_POINT('Ctrl Pts',(48.706329375,39.4791666734946,13.0508216223155));
#9819=CARTESIAN_POINT('Ctrl Pts',(42.1809185638422,39.2708333401613,24.3531646875));
#9820=CARTESIAN_POINT('Ctrl Pts',(35.6555077526845,39.062500006828,35.6555077526845));
#9821=CARTESIAN_POINT('Ctrl Pts',(24.3531646875,38.8541666734946,42.1809185638422));
#9822=CARTESIAN_POINT('Ctrl Pts',(13.0508216223155,38.6458333401613,48.706329375));
#9823=CARTESIAN_POINT('Ctrl Pts',(-9.95098946405443E-15,38.437500006828,
48.706329375));
#9824=CARTESIAN_POINT('Ctrl Pts',(-13.0508216223155,38.2291666734946,48.706329375));
#9825=CARTESIAN_POINT('Ctrl Pts',(-24.3531646875,38.0208333401613,42.1809185638423));
#9826=CARTESIAN_POINT('Ctrl Pts',(-35.6555077526845,37.812500006828,35.6555077526845));
#9827=CARTESIAN_POINT('Ctrl Pts',(-42.1809185638422,37.6041666734946,24.3531646875));
#9828=CARTESIAN_POINT('Ctrl Pts',(-48.706329375,37.3958333401613,13.0508216223155));
#9829=CARTESIAN_POINT('Ctrl Pts',(-48.706329375,37.187500006828,-1.8898197019151E-14));
#9830=CARTESIAN_POINT('Ctrl Pts',(-48.706329375,36.9791666734946,-13.0508216223155));
#9831=CARTESIAN_POINT('Ctrl Pts',(-42.1809185638422,36.7708333401613,-24.3531646875));
#9832=CARTESIAN_POINT('Ctrl Pts',(-35.6555077526845,36.562500006828,-35.6555077526845));
#9833=CARTESIAN_POINT('Ctrl Pts',(-24.3531646875,36.3541666734946,-42.1809185638423));
#9834=CARTESIAN_POINT('Ctrl Pts',(-13.0508216223155,36.1458333401613,-48.706329375));
#9835=CARTESIAN_POINT('Ctrl Pts',(1.59157945007855E-14,35.937500006828,
-48.706329375));
#9836=CARTESIAN_POINT('Ctrl Pts',(13.0508216223155,35.7291666734946,-48.706329375));
#9837=CARTESIAN_POINT('Ctrl Pts',(24.3531646875,35.5208333401613,-42.1809185638422));
#9838=CARTESIAN_POINT('Ctrl Pts',(35.6555077526845,35.312500006828,-35.6555077526845));
#9839=CARTESIAN_POINT('Ctrl Pts',(42.1809185638422,35.1041666734946,-24.3531646875));
#9840=CARTESIAN_POINT('Ctrl Pts',(48.706329375,34.8958333401613,-13.0508216223155));
#9841=CARTESIAN_POINT('Ctrl Pts',(48.706329375,34.687500006828,1.293339198242E-14));
#9842=CARTESIAN_POINT('Ctrl Pts',(48.706329375,34.4791666734946,13.0508216223155));
#9843=CARTESIAN_POINT('Ctrl Pts',(42.1809185638422,34.2708333401613,24.3531646875));
#9844=CARTESIAN_POINT('Ctrl Pts',(35.6555077526845,34.062500006828,35.6555077526845));
#9845=CARTESIAN_POINT('Ctrl Pts',(24.3531646875,33.8541666734946,42.1809185638422));
#9846=CARTESIAN_POINT('Ctrl Pts',(13.0508216223155,33.6458333401613,48.706329375));
#9847=CARTESIAN_POINT('Ctrl Pts',(-9.95098946405443E-15,33.437500006828,
48.706329375));
#9848=CARTESIAN_POINT('Ctrl Pts',(-13.0508216223155,33.2291666734946,48.706329375));
#9849=CARTESIAN_POINT('Ctrl Pts',(-24.3531646875,33.0208333401613,42.1809185638423));
#9850=CARTESIAN_POINT('Ctrl Pts',(-35.6555077526845,32.812500006828,35.6555077526845));
#9851=CARTESIAN_POINT('Ctrl Pts',(-42.1809185638422,32.6041666734946,24.3531646875));
#9852=CARTESIAN_POINT('Ctrl Pts',(-48.706329375,32.3958333401613,13.0508216223155));
#9853=CARTESIAN_POINT('Ctrl Pts',(-48.706329375,32.187500006828,-1.8898197019151E-14));
#9854=CARTESIAN_POINT('Ctrl Pts',(-48.706329375,31.9791666734946,-13.0508216223155));
#9855=CARTESIAN_POINT('Ctrl Pts',(-42.1809185638422,31.7708333401613,-24.3531646875));
#9856=CARTESIAN_POINT('Ctrl Pts',(-35.6555077526845,31.562500006828,-35.6555077526845));
#9857=CARTESIAN_POINT('Ctrl Pts',(-24.3531646875,31.3541666734946,-42.1809185638423));
#9858=CARTESIAN_POINT('Ctrl Pts',(-13.0508216223155,31.1458333401613,-48.706329375));
#9859=CARTESIAN_POINT('Ctrl Pts',(1.59157945007855E-14,30.937500006828,
-48.706329375));
#9860=CARTESIAN_POINT('Ctrl Pts',(13.0508216223155,30.7291666734946,-48.706329375));
#9861=CARTESIAN_POINT('Ctrl Pts',(24.3531646875,30.5208333401613,-42.1809185638422));
#9862=CARTESIAN_POINT('Ctrl Pts',(35.6555077526845,30.312500006828,-35.6555077526845));
#9863=CARTESIAN_POINT('Ctrl Pts',(42.1809185638422,30.1041666734946,-24.3531646875));
#9864=CARTESIAN_POINT('Ctrl Pts',(48.706329375,29.8958333401613,-13.0508216223155));
#9865=CARTESIAN_POINT('Ctrl Pts',(48.706329375,29.687500006828,1.293339198242E-14));
#9866=CARTESIAN_POINT('Ctrl Pts',(48.706329375,29.4791666734946,13.0508216223155));
#9867=CARTESIAN_POINT('Ctrl Pts',(42.1809185638422,29.2708333401613,24.3531646875));
#9868=CARTESIAN_POINT('Ctrl Pts',(35.6555077526845,29.062500006828,35.6555077526845));
#9869=CARTESIAN_POINT('Ctrl Pts',(24.3531646875,28.8541666734946,42.1809185638422));
#9870=CARTESIAN_POINT('Ctrl Pts',(13.0508216223155,28.6458333401613,48.706329375));
#9871=CARTESIAN_POINT('Ctrl Pts',(-9.95098946405443E-15,28.437500006828,
48.706329375));
#9872=CARTESIAN_POINT('Ctrl Pts',(-13.0508216223155,28.2291666734946,48.706329375));
#9873=CARTESIAN_POINT('Ctrl Pts',(-24.3531646875,28.0208333401613,42.1809185638423));
#9874=CARTESIAN_POINT('Ctrl Pts',(-35.6555077526845,27.812500006828,35.6555077526845));
#9875=CARTESIAN_POINT('Ctrl Pts',(-42.1809185638422,27.6041666734946,24.3531646875));
#9876=CARTESIAN_POINT('Ctrl Pts',(-48.706329375,27.3958333401613,13.0508216223155));
#9877=CARTESIAN_POINT('Ctrl Pts',(-48.706329375,27.187500006828,-1.8898197019151E-14));
#9878=CARTESIAN_POINT('',(-48.5134353784345,42.1175463684955,-4.33048599679665));
#9879=CARTESIAN_POINT('Ctrl Pts',(-45.7957082162897,40.5508791552084,-4.33048599679673));
#9880=CARTESIAN_POINT('Ctrl Pts',(-46.027322302781,40.6843839384496,-4.33048599679682));
#9881=CARTESIAN_POINT('Ctrl Pts',(-46.4905476657728,40.9513983799648,-4.33048599679661));
#9882=CARTESIAN_POINT('Ctrl Pts',(-46.9537676533565,41.2184221466352,-4.33048599679666));
#9883=CARTESIAN_POINT('Ctrl Pts',(-47.6280672732222,41.6071316973962,-4.33048599679666));
#9884=CARTESIAN_POINT('Ctrl Pts',(-48.0707534890442,41.8623352807796,-4.33048599679665));
#9885=CARTESIAN_POINT('Ctrl Pts',(-48.5134353784345,42.1175463684955,-4.33048599679665));
#9886=CARTESIAN_POINT('',(-4.32456003949873,41.0073567866782,-48.5139639861634));
#9887=CARTESIAN_POINT('Ctrl Pts',(-48.5134353784345,42.1175463684955,-4.33048599679665));
#9888=CARTESIAN_POINT('Ctrl Pts',(-47.5573898704235,41.9424850907233,-15.040843219065));
#9889=CARTESIAN_POINT('Ctrl Pts',(-42.1809185638422,41.7708333401613,-24.3531646875));
#9890=CARTESIAN_POINT('Ctrl Pts',(-35.6555077526845,41.562500006828,-35.6555077526845));
#9891=CARTESIAN_POINT('Ctrl Pts',(-24.3531646875,41.3541666734946,-42.1809185638423));
#9892=CARTESIAN_POINT('Ctrl Pts',(-15.038141415499,41.1824651212465,-47.5589497574396));
#9893=CARTESIAN_POINT('Ctrl Pts',(-4.32456003949873,41.0073567866782,-48.5139639861634));
#9894=CARTESIAN_POINT('Origin',(-4.32456091837631,8012.2045409659,4524.01087410016));
#9895=CARTESIAN_POINT('Ctrl Pts',(-46.,55.6250000136559,0.));
#9896=CARTESIAN_POINT('Ctrl Pts',(-46.,55.4166666803226,-12.3256628518316));
#9897=CARTESIAN_POINT('Ctrl Pts',(-39.8371685740842,55.2083333469893,-23.));
#9898=CARTESIAN_POINT('Ctrl Pts',(-33.6743371481684,55.0000000136559,-33.6743371481684));
#9899=CARTESIAN_POINT('Ctrl Pts',(-23.,54.7916666803226,-39.8371685740842));
#9900=CARTESIAN_POINT('Ctrl Pts',(-12.3256628518317,54.5833333469893,-46.));
#9901=CARTESIAN_POINT('Ctrl Pts',(-2.81668763803891E-15,54.3750000136559,
-46.));
#9902=CARTESIAN_POINT('Ctrl Pts',(12.3256628518316,54.1666666803226,-46.));
#9903=CARTESIAN_POINT('Ctrl Pts',(23.,53.9583333469893,-39.8371685740842));
#9904=CARTESIAN_POINT('Ctrl Pts',(33.6743371481683,53.7500000136559,-33.6743371481684));
#9905=CARTESIAN_POINT('Ctrl Pts',(39.8371685740842,53.5416666803226,-23.));
#9906=CARTESIAN_POINT('Ctrl Pts',(46.,53.3333333469893,-12.3256628518317));
#9907=CARTESIAN_POINT('Ctrl Pts',(46.,53.1250000136559,-5.63337527607782E-15));
#9908=CARTESIAN_POINT('Ctrl Pts',(46.,52.9166666803226,12.3256628518316));
#9909=CARTESIAN_POINT('Ctrl Pts',(39.8371685740842,52.7083333469893,23.));
#9910=CARTESIAN_POINT('Ctrl Pts',(33.6743371481684,52.5000000136559,33.6743371481683));
#9911=CARTESIAN_POINT('Ctrl Pts',(23.,52.2916666803226,39.8371685740842));
#9912=CARTESIAN_POINT('Ctrl Pts',(12.3256628518317,52.0833333469893,46.));
#9913=CARTESIAN_POINT('Ctrl Pts',(8.45006291411674E-15,51.8750000136559,
46.));
#9914=CARTESIAN_POINT('Ctrl Pts',(-12.3256628518316,51.6666666803226,46.));
#9915=CARTESIAN_POINT('Ctrl Pts',(-23.,51.4583333469893,39.8371685740842));
#9916=CARTESIAN_POINT('Ctrl Pts',(-33.6743371481683,51.2500000136559,33.6743371481684));
#9917=CARTESIAN_POINT('Ctrl Pts',(-39.8371685740842,51.0416666803226,23.));
#9918=CARTESIAN_POINT('Ctrl Pts',(-46.,50.8333333469893,12.3256628518317));
#9919=CARTESIAN_POINT('Ctrl Pts',(-46.,50.6250000136559,0.));
#9920=CARTESIAN_POINT('Ctrl Pts',(-46.,50.4166666803226,-12.3256628518316));
#9921=CARTESIAN_POINT('Ctrl Pts',(-39.8371685740842,50.2083333469893,-23.));
#9922=CARTESIAN_POINT('Ctrl Pts',(-33.6743371481684,50.0000000136559,-33.6743371481684));
#9923=CARTESIAN_POINT('Ctrl Pts',(-23.,49.7916666803226,-39.8371685740842));
#9924=CARTESIAN_POINT('Ctrl Pts',(-12.3256628518317,49.5833333469893,-46.));
#9925=CARTESIAN_POINT('Ctrl Pts',(-2.81668763803891E-15,49.3750000136559,
-46.));
#9926=CARTESIAN_POINT('Ctrl Pts',(12.3256628518316,49.1666666803226,-46.));
#9927=CARTESIAN_POINT('Ctrl Pts',(23.,48.9583333469893,-39.8371685740842));
#9928=CARTESIAN_POINT('Ctrl Pts',(33.6743371481683,48.7500000136559,-33.6743371481684));
#9929=CARTESIAN_POINT('Ctrl Pts',(39.8371685740842,48.5416666803226,-23.));
#9930=CARTESIAN_POINT('Ctrl Pts',(46.,48.3333333469893,-12.3256628518317));
#9931=CARTESIAN_POINT('Ctrl Pts',(46.,48.1250000136559,-5.63337527607782E-15));
#9932=CARTESIAN_POINT('Ctrl Pts',(46.,47.9166666803226,12.3256628518316));
#9933=CARTESIAN_POINT('Ctrl Pts',(39.8371685740842,47.7083333469893,23.));
#9934=CARTESIAN_POINT('Ctrl Pts',(33.6743371481684,47.5000000136559,33.6743371481683));
#9935=CARTESIAN_POINT('Ctrl Pts',(23.,47.2916666803226,39.8371685740842));
#9936=CARTESIAN_POINT('Ctrl Pts',(12.3256628518317,47.0833333469893,46.));
#9937=CARTESIAN_POINT('Ctrl Pts',(8.45006291411674E-15,46.8750000136559,
46.));
#9938=CARTESIAN_POINT('Ctrl Pts',(-12.3256628518316,46.6666666803226,46.));
#9939=CARTESIAN_POINT('Ctrl Pts',(-23.,46.4583333469893,39.8371685740842));
#9940=CARTESIAN_POINT('Ctrl Pts',(-33.6743371481683,46.2500000136559,33.6743371481684));
#9941=CARTESIAN_POINT('Ctrl Pts',(-39.8371685740842,46.0416666803226,23.));
#9942=CARTESIAN_POINT('Ctrl Pts',(-46.,45.8333333469892,12.3256628518317));
#9943=CARTESIAN_POINT('Ctrl Pts',(-46.,45.6250000136559,0.));
#9944=CARTESIAN_POINT('Ctrl Pts',(-46.,45.4166666803226,-12.3256628518316));
#9945=CARTESIAN_POINT('Ctrl Pts',(-39.8371685740842,45.2083333469893,-23.));
#9946=CARTESIAN_POINT('Ctrl Pts',(-33.6743371481684,45.0000000136559,-33.6743371481684));
#9947=CARTESIAN_POINT('Ctrl Pts',(-23.,44.7916666803226,-39.8371685740842));
#9948=CARTESIAN_POINT('Ctrl Pts',(-12.3256628518317,44.5833333469893,-46.));
#9949=CARTESIAN_POINT('Ctrl Pts',(-2.81668763803891E-15,44.3750000136559,
-46.));
#9950=CARTESIAN_POINT('Ctrl Pts',(12.3256628518316,44.1666666803226,-46.));
#9951=CARTESIAN_POINT('Ctrl Pts',(23.,43.9583333469893,-39.8371685740842));
#9952=CARTESIAN_POINT('Ctrl Pts',(33.6743371481683,43.7500000136559,-33.6743371481684));
#9953=CARTESIAN_POINT('Ctrl Pts',(39.8371685740842,43.5416666803226,-23.));
#9954=CARTESIAN_POINT('Ctrl Pts',(46.,43.3333333469893,-12.3256628518317));
#9955=CARTESIAN_POINT('Ctrl Pts',(46.,43.1250000136559,-5.63337527607782E-15));
#9956=CARTESIAN_POINT('Ctrl Pts',(46.,42.9166666803226,12.3256628518316));
#9957=CARTESIAN_POINT('Ctrl Pts',(39.8371685740842,42.7083333469893,23.));
#9958=CARTESIAN_POINT('Ctrl Pts',(33.6743371481684,42.5000000136559,33.6743371481683));
#9959=CARTESIAN_POINT('Ctrl Pts',(23.,42.2916666803226,39.8371685740842));
#9960=CARTESIAN_POINT('Ctrl Pts',(12.3256628518317,42.0833333469893,46.));
#9961=CARTESIAN_POINT('Ctrl Pts',(8.45006291411674E-15,41.8750000136559,
46.));
#9962=CARTESIAN_POINT('Ctrl Pts',(-12.3256628518316,41.6666666803226,46.));
#9963=CARTESIAN_POINT('Ctrl Pts',(-23.,41.4583333469893,39.8371685740842));
#9964=CARTESIAN_POINT('Ctrl Pts',(-33.6743371481683,41.2500000136559,33.6743371481684));
#9965=CARTESIAN_POINT('Ctrl Pts',(-39.8371685740842,41.0416666803226,23.));
#9966=CARTESIAN_POINT('Ctrl Pts',(-46.,40.8333333469893,12.3256628518317));
#9967=CARTESIAN_POINT('Ctrl Pts',(-46.,40.6250000136559,0.));
#9968=CARTESIAN_POINT('Ctrl Pts',(-46.,40.4166666803226,-12.3256628518316));
#9969=CARTESIAN_POINT('Ctrl Pts',(-39.8371685740842,40.2083333469893,-23.));
#9970=CARTESIAN_POINT('Ctrl Pts',(-33.6743371481684,40.0000000136559,-33.6743371481684));
#9971=CARTESIAN_POINT('Ctrl Pts',(-23.,39.7916666803226,-39.8371685740842));
#9972=CARTESIAN_POINT('Ctrl Pts',(-12.3256628518317,39.5833333469893,-46.));
#9973=CARTESIAN_POINT('Ctrl Pts',(-2.81668763803891E-15,39.3750000136559,
-46.));
#9974=CARTESIAN_POINT('Ctrl Pts',(12.3256628518316,39.1666666803226,-46.));
#9975=CARTESIAN_POINT('Ctrl Pts',(23.,38.9583333469893,-39.8371685740842));
#9976=CARTESIAN_POINT('Ctrl Pts',(33.6743371481683,38.7500000136559,-33.6743371481684));
#9977=CARTESIAN_POINT('Ctrl Pts',(39.8371685740842,38.5416666803226,-23.));
#9978=CARTESIAN_POINT('Ctrl Pts',(46.,38.3333333469893,-12.3256628518317));
#9979=CARTESIAN_POINT('Ctrl Pts',(46.,38.1250000136559,-5.63337527607782E-15));
#9980=CARTESIAN_POINT('Ctrl Pts',(46.,37.9166666803226,12.3256628518316));
#9981=CARTESIAN_POINT('Ctrl Pts',(39.8371685740842,37.7083333469893,23.));
#9982=CARTESIAN_POINT('Ctrl Pts',(33.6743371481684,37.5000000136559,33.6743371481683));
#9983=CARTESIAN_POINT('Ctrl Pts',(23.,37.2916666803226,39.8371685740842));
#9984=CARTESIAN_POINT('Ctrl Pts',(12.3256628518317,37.0833333469893,46.));
#9985=CARTESIAN_POINT('Ctrl Pts',(8.45006291411674E-15,36.8750000136559,
46.));
#9986=CARTESIAN_POINT('Ctrl Pts',(-12.3256628518316,36.6666666803226,46.));
#9987=CARTESIAN_POINT('Ctrl Pts',(-23.,36.4583333469893,39.8371685740842));
#9988=CARTESIAN_POINT('Ctrl Pts',(-33.6743371481683,36.2500000136559,33.6743371481684));
#9989=CARTESIAN_POINT('Ctrl Pts',(-39.8371685740842,36.0416666803226,23.));
#9990=CARTESIAN_POINT('Ctrl Pts',(-46.,35.8333333469893,12.3256628518317));
#9991=CARTESIAN_POINT('Ctrl Pts',(-46.,35.6250000136559,0.));
#9992=CARTESIAN_POINT('Ctrl Pts',(-46.,35.4166666803226,-12.3256628518316));
#9993=CARTESIAN_POINT('Ctrl Pts',(-39.8371685740842,35.2083333469893,-23.));
#9994=CARTESIAN_POINT('Ctrl Pts',(-33.6743371481684,35.0000000136559,-33.6743371481684));
#9995=CARTESIAN_POINT('Ctrl Pts',(-23.,34.7916666803226,-39.8371685740842));
#9996=CARTESIAN_POINT('Ctrl Pts',(-12.3256628518317,34.5833333469893,-46.));
#9997=CARTESIAN_POINT('Ctrl Pts',(-2.81668763803891E-15,34.3750000136559,
-46.));
#9998=CARTESIAN_POINT('Ctrl Pts',(12.3256628518316,34.1666666803226,-46.));
#9999=CARTESIAN_POINT('Ctrl Pts',(23.,33.9583333469893,-39.8371685740842));
#10000=CARTESIAN_POINT('Ctrl Pts',(33.6743371481683,33.7500000136559,-33.6743371481684));
#10001=CARTESIAN_POINT('Ctrl Pts',(39.8371685740842,33.5416666803226,-23.));
#10002=CARTESIAN_POINT('Ctrl Pts',(46.,33.3333333469893,-12.3256628518317));
#10003=CARTESIAN_POINT('Ctrl Pts',(46.,33.1250000136559,-5.63337527607782E-15));
#10004=CARTESIAN_POINT('Ctrl Pts',(46.,32.9166666803226,12.3256628518316));
#10005=CARTESIAN_POINT('Ctrl Pts',(39.8371685740842,32.7083333469893,23.));
#10006=CARTESIAN_POINT('Ctrl Pts',(33.6743371481684,32.5000000136559,33.6743371481683));
#10007=CARTESIAN_POINT('Ctrl Pts',(23.,32.2916666803226,39.8371685740842));
#10008=CARTESIAN_POINT('Ctrl Pts',(12.3256628518317,32.0833333469893,46.));
#10009=CARTESIAN_POINT('Ctrl Pts',(8.45006291411674E-15,31.8750000136559,
46.));
#10010=CARTESIAN_POINT('Ctrl Pts',(-12.3256628518316,31.6666666803226,46.));
#10011=CARTESIAN_POINT('Ctrl Pts',(-23.,31.4583333469893,39.8371685740842));
#10012=CARTESIAN_POINT('Ctrl Pts',(-33.6743371481683,31.2500000136559,33.6743371481684));
#10013=CARTESIAN_POINT('Ctrl Pts',(-39.8371685740842,31.0416666803226,23.));
#10014=CARTESIAN_POINT('Ctrl Pts',(-46.,30.8333333469893,12.3256628518317));
#10015=CARTESIAN_POINT('Ctrl Pts',(-46.,30.6250000136559,0.));
#10016=CARTESIAN_POINT('Ctrl Pts',(-46.,30.4166666803226,-12.3256628518316));
#10017=CARTESIAN_POINT('Ctrl Pts',(-39.8371685740842,30.2083333469893,-23.));
#10018=CARTESIAN_POINT('Ctrl Pts',(-33.6743371481684,30.0000000136559,-33.6743371481684));
#10019=CARTESIAN_POINT('Ctrl Pts',(-23.,29.7916666803226,-39.8371685740842));
#10020=CARTESIAN_POINT('Ctrl Pts',(-12.3256628518317,29.5833333469893,-46.));
#10021=CARTESIAN_POINT('Ctrl Pts',(-2.81668763803891E-15,29.3750000136559,
-46.));
#10022=CARTESIAN_POINT('Ctrl Pts',(12.3256628518316,29.1666666803226,-46.));
#10023=CARTESIAN_POINT('Ctrl Pts',(23.,28.9583333469893,-39.8371685740842));
#10024=CARTESIAN_POINT('Ctrl Pts',(33.6743371481683,28.7500000136559,-33.6743371481684));
#10025=CARTESIAN_POINT('Ctrl Pts',(39.8371685740842,28.5416666803226,-23.));
#10026=CARTESIAN_POINT('Ctrl Pts',(46.,28.3333333469893,-12.3256628518317));
#10027=CARTESIAN_POINT('Ctrl Pts',(46.,28.1250000136559,-5.63337527607782E-15));
#10028=CARTESIAN_POINT('Ctrl Pts',(46.,27.9166666803226,12.3256628518316));
#10029=CARTESIAN_POINT('Ctrl Pts',(39.8371685740842,27.7083333469893,23.));
#10030=CARTESIAN_POINT('Ctrl Pts',(33.6743371481684,27.5000000136559,33.6743371481683));
#10031=CARTESIAN_POINT('Ctrl Pts',(23.,27.2916666803226,39.8371685740842));
#10032=CARTESIAN_POINT('Ctrl Pts',(12.3256628518317,27.0833333469893,46.));
#10033=CARTESIAN_POINT('Ctrl Pts',(8.45006291411674E-15,26.8750000136559,
46.));
#10034=CARTESIAN_POINT('Ctrl Pts',(-12.3256628518316,26.6666666803226,46.));
#10035=CARTESIAN_POINT('Ctrl Pts',(-23.,26.4583333469893,39.8371685740842));
#10036=CARTESIAN_POINT('Ctrl Pts',(-33.6743371481683,26.2500000136559,33.6743371481684));
#10037=CARTESIAN_POINT('Ctrl Pts',(-39.8371685740842,26.0416666803226,23.));
#10038=CARTESIAN_POINT('Ctrl Pts',(-46.,25.8333333469893,12.3256628518317));
#10039=CARTESIAN_POINT('Ctrl Pts',(-46.,25.6250000136559,0.));
#10040=CARTESIAN_POINT('Ctrl Pts',(-48.706329375,57.187500006828,-1.8898197019151E-14));
#10041=CARTESIAN_POINT('Ctrl Pts',(-48.706329375,56.9791666734946,-13.0508216223155));
#10042=CARTESIAN_POINT('Ctrl Pts',(-42.1809185638422,56.7708333401613,-24.3531646875));
#10043=CARTESIAN_POINT('Ctrl Pts',(-35.6555077526845,56.562500006828,-35.6555077526845));
#10044=CARTESIAN_POINT('Ctrl Pts',(-24.3531646875,56.3541666734946,-42.1809185638423));
#10045=CARTESIAN_POINT('Ctrl Pts',(-13.0508216223155,56.1458333401613,-48.706329375));
#10046=CARTESIAN_POINT('Ctrl Pts',(1.59157945007855E-14,55.937500006828,
-48.706329375));
#10047=CARTESIAN_POINT('Ctrl Pts',(13.0508216223155,55.7291666734946,-48.706329375));
#10048=CARTESIAN_POINT('Ctrl Pts',(24.3531646875,55.5208333401613,-42.1809185638422));
#10049=CARTESIAN_POINT('Ctrl Pts',(35.6555077526845,55.312500006828,-35.6555077526845));
#10050=CARTESIAN_POINT('Ctrl Pts',(42.1809185638422,55.1041666734946,-24.3531646875));
#10051=CARTESIAN_POINT('Ctrl Pts',(48.706329375,54.8958333401613,-13.0508216223155));
#10052=CARTESIAN_POINT('Ctrl Pts',(48.706329375,54.687500006828,1.293339198242E-14));
#10053=CARTESIAN_POINT('Ctrl Pts',(48.706329375,54.4791666734946,13.0508216223155));
#10054=CARTESIAN_POINT('Ctrl Pts',(42.1809185638422,54.2708333401613,24.3531646875));
#10055=CARTESIAN_POINT('Ctrl Pts',(35.6555077526845,54.062500006828,35.6555077526845));
#10056=CARTESIAN_POINT('Ctrl Pts',(24.3531646875,53.8541666734946,42.1809185638422));
#10057=CARTESIAN_POINT('Ctrl Pts',(13.0508216223155,53.6458333401613,48.706329375));
#10058=CARTESIAN_POINT('Ctrl Pts',(-9.95098946405443E-15,53.437500006828,
48.706329375));
#10059=CARTESIAN_POINT('Ctrl Pts',(-13.0508216223155,53.2291666734946,48.706329375));
#10060=CARTESIAN_POINT('Ctrl Pts',(-24.3531646875,53.0208333401613,42.1809185638423));
#10061=CARTESIAN_POINT('Ctrl Pts',(-35.6555077526845,52.812500006828,35.6555077526845));
#10062=CARTESIAN_POINT('Ctrl Pts',(-42.1809185638422,52.6041666734946,24.3531646875));
#10063=CARTESIAN_POINT('Ctrl Pts',(-48.706329375,52.3958333401613,13.0508216223155));
#10064=CARTESIAN_POINT('Ctrl Pts',(-48.706329375,52.187500006828,-1.8898197019151E-14));
#10065=CARTESIAN_POINT('Ctrl Pts',(-48.706329375,51.9791666734946,-13.0508216223155));
#10066=CARTESIAN_POINT('Ctrl Pts',(-42.1809185638422,51.7708333401613,-24.3531646875));
#10067=CARTESIAN_POINT('Ctrl Pts',(-35.6555077526845,51.562500006828,-35.6555077526845));
#10068=CARTESIAN_POINT('Ctrl Pts',(-24.3531646875,51.3541666734946,-42.1809185638423));
#10069=CARTESIAN_POINT('Ctrl Pts',(-13.0508216223155,51.1458333401613,-48.706329375));
#10070=CARTESIAN_POINT('Ctrl Pts',(1.59157945007855E-14,50.937500006828,
-48.706329375));
#10071=CARTESIAN_POINT('Ctrl Pts',(13.0508216223155,50.7291666734946,-48.706329375));
#10072=CARTESIAN_POINT('Ctrl Pts',(24.3531646875,50.5208333401613,-42.1809185638422));
#10073=CARTESIAN_POINT('Ctrl Pts',(35.6555077526845,50.312500006828,-35.6555077526845));
#10074=CARTESIAN_POINT('Ctrl Pts',(42.1809185638422,50.1041666734946,-24.3531646875));
#10075=CARTESIAN_POINT('Ctrl Pts',(48.706329375,49.8958333401613,-13.0508216223155));
#10076=CARTESIAN_POINT('Ctrl Pts',(48.706329375,49.687500006828,1.293339198242E-14));
#10077=CARTESIAN_POINT('Ctrl Pts',(48.706329375,49.4791666734946,13.0508216223155));
#10078=CARTESIAN_POINT('Ctrl Pts',(42.1809185638422,49.2708333401613,24.3531646875));
#10079=CARTESIAN_POINT('Ctrl Pts',(35.6555077526845,49.062500006828,35.6555077526845));
#10080=CARTESIAN_POINT('Ctrl Pts',(24.3531646875,48.8541666734946,42.1809185638422));
#10081=CARTESIAN_POINT('Ctrl Pts',(13.0508216223155,48.6458333401613,48.706329375));
#10082=CARTESIAN_POINT('Ctrl Pts',(-9.95098946405443E-15,48.437500006828,
48.706329375));
#10083=CARTESIAN_POINT('Ctrl Pts',(-13.0508216223155,48.2291666734946,48.706329375));
#10084=CARTESIAN_POINT('Ctrl Pts',(-24.3531646875,48.0208333401613,42.1809185638423));
#10085=CARTESIAN_POINT('Ctrl Pts',(-35.6555077526845,47.812500006828,35.6555077526845));
#10086=CARTESIAN_POINT('Ctrl Pts',(-42.1809185638422,47.6041666734946,24.3531646875));
#10087=CARTESIAN_POINT('Ctrl Pts',(-48.706329375,47.3958333401613,13.0508216223155));
#10088=CARTESIAN_POINT('Ctrl Pts',(-48.706329375,47.187500006828,-1.8898197019151E-14));
#10089=CARTESIAN_POINT('Ctrl Pts',(-48.706329375,46.9791666734946,-13.0508216223155));
#10090=CARTESIAN_POINT('Ctrl Pts',(-42.1809185638422,46.7708333401613,-24.3531646875));
#10091=CARTESIAN_POINT('Ctrl Pts',(-35.6555077526845,46.562500006828,-35.6555077526845));
#10092=CARTESIAN_POINT('Ctrl Pts',(-24.3531646875,46.3541666734946,-42.1809185638423));
#10093=CARTESIAN_POINT('Ctrl Pts',(-13.0508216223155,46.1458333401613,-48.706329375));
#10094=CARTESIAN_POINT('Ctrl Pts',(1.59157945007855E-14,45.937500006828,
-48.706329375));
#10095=CARTESIAN_POINT('Ctrl Pts',(13.0508216223155,45.7291666734946,-48.706329375));
#10096=CARTESIAN_POINT('Ctrl Pts',(24.3531646875,45.5208333401613,-42.1809185638422));
#10097=CARTESIAN_POINT('Ctrl Pts',(35.6555077526845,45.312500006828,-35.6555077526845));
#10098=CARTESIAN_POINT('Ctrl Pts',(42.1809185638422,45.1041666734946,-24.3531646875));
#10099=CARTESIAN_POINT('Ctrl Pts',(48.706329375,44.8958333401613,-13.0508216223155));
#10100=CARTESIAN_POINT('Ctrl Pts',(48.706329375,44.687500006828,1.293339198242E-14));
#10101=CARTESIAN_POINT('Ctrl Pts',(48.706329375,44.4791666734946,13.0508216223155));
#10102=CARTESIAN_POINT('Ctrl Pts',(42.1809185638422,44.2708333401613,24.3531646875));
#10103=CARTESIAN_POINT('Ctrl Pts',(35.6555077526845,44.062500006828,35.6555077526845));
#10104=CARTESIAN_POINT('Ctrl Pts',(24.3531646875,43.8541666734946,42.1809185638422));
#10105=CARTESIAN_POINT('Ctrl Pts',(13.0508216223155,43.6458333401613,48.706329375));
#10106=CARTESIAN_POINT('Ctrl Pts',(-9.95098946405443E-15,43.437500006828,
48.706329375));
#10107=CARTESIAN_POINT('Ctrl Pts',(-13.0508216223155,43.2291666734946,48.706329375));
#10108=CARTESIAN_POINT('Ctrl Pts',(-24.3531646875,43.0208333401613,42.1809185638423));
#10109=CARTESIAN_POINT('Ctrl Pts',(-35.6555077526845,42.812500006828,35.6555077526845));
#10110=CARTESIAN_POINT('Ctrl Pts',(-42.1809185638422,42.6041666734946,24.3531646875));
#10111=CARTESIAN_POINT('Ctrl Pts',(-48.706329375,42.3958333401613,13.0508216223155));
#10112=CARTESIAN_POINT('Ctrl Pts',(-48.706329375,42.187500006828,-1.8898197019151E-14));
#10113=CARTESIAN_POINT('Ctrl Pts',(-48.706329375,41.9791666734946,-13.0508216223155));
#10114=CARTESIAN_POINT('Ctrl Pts',(-42.1809185638422,41.7708333401613,-24.3531646875));
#10115=CARTESIAN_POINT('Ctrl Pts',(-35.6555077526845,41.562500006828,-35.6555077526845));
#10116=CARTESIAN_POINT('Ctrl Pts',(-24.3531646875,41.3541666734946,-42.1809185638423));
#10117=CARTESIAN_POINT('Ctrl Pts',(-13.0508216223155,41.1458333401613,-48.706329375));
#10118=CARTESIAN_POINT('Ctrl Pts',(1.59157945007855E-14,40.937500006828,
-48.706329375));
#10119=CARTESIAN_POINT('Ctrl Pts',(13.0508216223155,40.7291666734946,-48.706329375));
#10120=CARTESIAN_POINT('Ctrl Pts',(24.3531646875,40.5208333401613,-42.1809185638422));
#10121=CARTESIAN_POINT('Ctrl Pts',(35.6555077526845,40.312500006828,-35.6555077526845));
#10122=CARTESIAN_POINT('Ctrl Pts',(42.1809185638422,40.1041666734946,-24.3531646875));
#10123=CARTESIAN_POINT('Ctrl Pts',(48.706329375,39.8958333401613,-13.0508216223155));
#10124=CARTESIAN_POINT('Ctrl Pts',(48.706329375,39.687500006828,1.293339198242E-14));
#10125=CARTESIAN_POINT('Ctrl Pts',(48.706329375,39.4791666734946,13.0508216223155));
#10126=CARTESIAN_POINT('Ctrl Pts',(42.1809185638422,39.2708333401613,24.3531646875));
#10127=CARTESIAN_POINT('Ctrl Pts',(35.6555077526845,39.062500006828,35.6555077526845));
#10128=CARTESIAN_POINT('Ctrl Pts',(24.3531646875,38.8541666734946,42.1809185638422));
#10129=CARTESIAN_POINT('Ctrl Pts',(13.0508216223155,38.6458333401613,48.706329375));
#10130=CARTESIAN_POINT('Ctrl Pts',(-9.95098946405443E-15,38.437500006828,
48.706329375));
#10131=CARTESIAN_POINT('Ctrl Pts',(-13.0508216223155,38.2291666734946,48.706329375));
#10132=CARTESIAN_POINT('Ctrl Pts',(-24.3531646875,38.0208333401613,42.1809185638423));
#10133=CARTESIAN_POINT('Ctrl Pts',(-35.6555077526845,37.812500006828,35.6555077526845));
#10134=CARTESIAN_POINT('Ctrl Pts',(-42.1809185638422,37.6041666734946,24.3531646875));
#10135=CARTESIAN_POINT('Ctrl Pts',(-48.706329375,37.3958333401613,13.0508216223155));
#10136=CARTESIAN_POINT('Ctrl Pts',(-48.706329375,37.187500006828,-1.8898197019151E-14));
#10137=CARTESIAN_POINT('Ctrl Pts',(-48.706329375,36.9791666734946,-13.0508216223155));
#10138=CARTESIAN_POINT('Ctrl Pts',(-42.1809185638422,36.7708333401613,-24.3531646875));
#10139=CARTESIAN_POINT('Ctrl Pts',(-35.6555077526845,36.562500006828,-35.6555077526845));
#10140=CARTESIAN_POINT('Ctrl Pts',(-24.3531646875,36.3541666734946,-42.1809185638423));
#10141=CARTESIAN_POINT('Ctrl Pts',(-13.0508216223155,36.1458333401613,-48.706329375));
#10142=CARTESIAN_POINT('Ctrl Pts',(1.59157945007855E-14,35.937500006828,
-48.706329375));
#10143=CARTESIAN_POINT('Ctrl Pts',(13.0508216223155,35.7291666734946,-48.706329375));
#10144=CARTESIAN_POINT('Ctrl Pts',(24.3531646875,35.5208333401613,-42.1809185638422));
#10145=CARTESIAN_POINT('Ctrl Pts',(35.6555077526845,35.312500006828,-35.6555077526845));
#10146=CARTESIAN_POINT('Ctrl Pts',(42.1809185638422,35.1041666734946,-24.3531646875));
#10147=CARTESIAN_POINT('Ctrl Pts',(48.706329375,34.8958333401613,-13.0508216223155));
#10148=CARTESIAN_POINT('Ctrl Pts',(48.706329375,34.687500006828,1.293339198242E-14));
#10149=CARTESIAN_POINT('Ctrl Pts',(48.706329375,34.4791666734946,13.0508216223155));
#10150=CARTESIAN_POINT('Ctrl Pts',(42.1809185638422,34.2708333401613,24.3531646875));
#10151=CARTESIAN_POINT('Ctrl Pts',(35.6555077526845,34.062500006828,35.6555077526845));
#10152=CARTESIAN_POINT('Ctrl Pts',(24.3531646875,33.8541666734946,42.1809185638422));
#10153=CARTESIAN_POINT('Ctrl Pts',(13.0508216223155,33.6458333401613,48.706329375));
#10154=CARTESIAN_POINT('Ctrl Pts',(-9.95098946405443E-15,33.437500006828,
48.706329375));
#10155=CARTESIAN_POINT('Ctrl Pts',(-13.0508216223155,33.2291666734946,48.706329375));
#10156=CARTESIAN_POINT('Ctrl Pts',(-24.3531646875,33.0208333401613,42.1809185638423));
#10157=CARTESIAN_POINT('Ctrl Pts',(-35.6555077526845,32.812500006828,35.6555077526845));
#10158=CARTESIAN_POINT('Ctrl Pts',(-42.1809185638422,32.6041666734946,24.3531646875));
#10159=CARTESIAN_POINT('Ctrl Pts',(-48.706329375,32.3958333401613,13.0508216223155));
#10160=CARTESIAN_POINT('Ctrl Pts',(-48.706329375,32.187500006828,-1.8898197019151E-14));
#10161=CARTESIAN_POINT('Ctrl Pts',(-48.706329375,31.9791666734946,-13.0508216223155));
#10162=CARTESIAN_POINT('Ctrl Pts',(-42.1809185638422,31.7708333401613,-24.3531646875));
#10163=CARTESIAN_POINT('Ctrl Pts',(-35.6555077526845,31.562500006828,-35.6555077526845));
#10164=CARTESIAN_POINT('Ctrl Pts',(-24.3531646875,31.3541666734946,-42.1809185638423));
#10165=CARTESIAN_POINT('Ctrl Pts',(-13.0508216223155,31.1458333401613,-48.706329375));
#10166=CARTESIAN_POINT('Ctrl Pts',(1.59157945007855E-14,30.937500006828,
-48.706329375));
#10167=CARTESIAN_POINT('Ctrl Pts',(13.0508216223155,30.7291666734946,-48.706329375));
#10168=CARTESIAN_POINT('Ctrl Pts',(24.3531646875,30.5208333401613,-42.1809185638422));
#10169=CARTESIAN_POINT('Ctrl Pts',(35.6555077526845,30.312500006828,-35.6555077526845));
#10170=CARTESIAN_POINT('Ctrl Pts',(42.1809185638422,30.1041666734946,-24.3531646875));
#10171=CARTESIAN_POINT('Ctrl Pts',(48.706329375,29.8958333401613,-13.0508216223155));
#10172=CARTESIAN_POINT('Ctrl Pts',(48.706329375,29.687500006828,1.293339198242E-14));
#10173=CARTESIAN_POINT('Ctrl Pts',(48.706329375,29.4791666734946,13.0508216223155));
#10174=CARTESIAN_POINT('Ctrl Pts',(42.1809185638422,29.2708333401613,24.3531646875));
#10175=CARTESIAN_POINT('Ctrl Pts',(35.6555077526845,29.062500006828,35.6555077526845));
#10176=CARTESIAN_POINT('Ctrl Pts',(24.3531646875,28.8541666734946,42.1809185638422));
#10177=CARTESIAN_POINT('Ctrl Pts',(13.0508216223155,28.6458333401613,48.706329375));
#10178=CARTESIAN_POINT('Ctrl Pts',(-9.95098946405443E-15,28.437500006828,
48.706329375));
#10179=CARTESIAN_POINT('Ctrl Pts',(-13.0508216223155,28.2291666734946,48.706329375));
#10180=CARTESIAN_POINT('Ctrl Pts',(-24.3531646875,28.0208333401613,42.1809185638423));
#10181=CARTESIAN_POINT('Ctrl Pts',(-35.6555077526845,27.812500006828,35.6555077526845));
#10182=CARTESIAN_POINT('Ctrl Pts',(-42.1809185638422,27.6041666734946,24.3531646875));
#10183=CARTESIAN_POINT('Ctrl Pts',(-48.706329375,27.3958333401613,13.0508216223155));
#10184=CARTESIAN_POINT('Ctrl Pts',(-48.706329375,27.187500006828,-1.8898197019151E-14));
#10185=CARTESIAN_POINT('',(-4.32456003949883,43.3676432269777,48.5139639861634));
#10186=CARTESIAN_POINT('',(-48.5725845633798,42.2456516907297,3.60701400320326));
#10187=CARTESIAN_POINT('Ctrl Pts',(-4.32456003949883,43.3676432269777,48.5139639861634));
#10188=CARTESIAN_POINT('Ctrl Pts',(-15.0381414154991,43.1925348924095,47.5589497574396));
#10189=CARTESIAN_POINT('Ctrl Pts',(-24.3531646875,43.0208333401613,42.1809185638423));
#10190=CARTESIAN_POINT('Ctrl Pts',(-35.6555077526845,42.812500006828,35.6555077526845));
#10191=CARTESIAN_POINT('Ctrl Pts',(-42.1809185638422,42.6041666734946,24.3531646875));
#10192=CARTESIAN_POINT('Ctrl Pts',(-47.7480251419552,42.4264286116308,14.7106532430575));
#10193=CARTESIAN_POINT('Ctrl Pts',(-48.5725845633798,42.2456516907297,3.60701400320326));
#10194=CARTESIAN_POINT('Ctrl Pts',(-48.5725845633798,42.2456516907297,3.60701400320326));
#10195=CARTESIAN_POINT('Ctrl Pts',(-48.3407853679392,42.1124685639422,3.60701400320326));
#10196=CARTESIAN_POINT('Ctrl Pts',(-48.1089821836664,41.9792923792741,3.60701400320326));
#10197=CARTESIAN_POINT('Ctrl Pts',(-47.6453674864979,41.7129545080418,3.60701400320326));
#10198=CARTESIAN_POINT('Ctrl Pts',(-47.4135559734253,41.5797928212585,3.60701400320325));
#10199=CARTESIAN_POINT('Ctrl Pts',(-47.1817401099609,41.4466387085919,3.60701400320325));
#10200=CARTESIAN_POINT('Ctrl Pts',(-46.7406305897488,41.1932671494809,3.60701400320325));
#10201=CARTESIAN_POINT('Ctrl Pts',(-46.2995053259033,40.9399229970588,3.60701400320326));
#10202=CARTESIAN_POINT('Ctrl Pts',(-45.858362923034,40.686608693912,3.60701400320327));
#10203=CARTESIAN_POINT('Ctrl Pts',(-4.32456003949882,41.8009818542622,45.7962681936506));
#10204=CARTESIAN_POINT('Ctrl Pts',(-4.32456003949882,41.9344874667937,46.0278818021281));
#10205=CARTESIAN_POINT('Ctrl Pts',(-4.3245600394987,42.2015035419424,46.4911062234486));
#10206=CARTESIAN_POINT('Ctrl Pts',(-4.32456003949883,42.4685288945405,46.954325296818));
#10207=CARTESIAN_POINT('Ctrl Pts',(-4.32456003949883,42.8572357107336,47.6286149142205));
#10208=CARTESIAN_POINT('Ctrl Pts',(-4.32456003949883,43.1124357360102,48.0712916022845));
#10209=CARTESIAN_POINT('Ctrl Pts',(-4.32456003949883,43.3676432269777,48.5139639861634));
#10210=CARTESIAN_POINT('Ctrl Pts',(-46.,55.6250000136559,0.));
#10211=CARTESIAN_POINT('Ctrl Pts',(-46.,55.4166666803226,-12.3256628518316));
#10212=CARTESIAN_POINT('Ctrl Pts',(-39.8371685740842,55.2083333469893,-23.));
#10213=CARTESIAN_POINT('Ctrl Pts',(-33.6743371481684,55.0000000136559,-33.6743371481684));
#10214=CARTESIAN_POINT('Ctrl Pts',(-23.,54.7916666803226,-39.8371685740842));
#10215=CARTESIAN_POINT('Ctrl Pts',(-12.3256628518317,54.5833333469893,-46.));
#10216=CARTESIAN_POINT('Ctrl Pts',(-2.81668763803891E-15,54.3750000136559,
-46.));
#10217=CARTESIAN_POINT('Ctrl Pts',(12.3256628518316,54.1666666803226,-46.));
#10218=CARTESIAN_POINT('Ctrl Pts',(23.,53.9583333469893,-39.8371685740842));
#10219=CARTESIAN_POINT('Ctrl Pts',(33.6743371481683,53.7500000136559,-33.6743371481684));
#10220=CARTESIAN_POINT('Ctrl Pts',(39.8371685740842,53.5416666803226,-23.));
#10221=CARTESIAN_POINT('Ctrl Pts',(46.,53.3333333469893,-12.3256628518317));
#10222=CARTESIAN_POINT('Ctrl Pts',(46.,53.1250000136559,-5.63337527607782E-15));
#10223=CARTESIAN_POINT('Ctrl Pts',(46.,52.9166666803226,12.3256628518316));
#10224=CARTESIAN_POINT('Ctrl Pts',(39.8371685740842,52.7083333469893,23.));
#10225=CARTESIAN_POINT('Ctrl Pts',(33.6743371481684,52.5000000136559,33.6743371481683));
#10226=CARTESIAN_POINT('Ctrl Pts',(23.,52.2916666803226,39.8371685740842));
#10227=CARTESIAN_POINT('Ctrl Pts',(12.3256628518317,52.0833333469893,46.));
#10228=CARTESIAN_POINT('Ctrl Pts',(8.45006291411674E-15,51.8750000136559,
46.));
#10229=CARTESIAN_POINT('Ctrl Pts',(-12.3256628518316,51.6666666803226,46.));
#10230=CARTESIAN_POINT('Ctrl Pts',(-23.,51.4583333469893,39.8371685740842));
#10231=CARTESIAN_POINT('Ctrl Pts',(-33.6743371481683,51.2500000136559,33.6743371481684));
#10232=CARTESIAN_POINT('Ctrl Pts',(-39.8371685740842,51.0416666803226,23.));
#10233=CARTESIAN_POINT('Ctrl Pts',(-46.,50.8333333469893,12.3256628518317));
#10234=CARTESIAN_POINT('Ctrl Pts',(-46.,50.6250000136559,0.));
#10235=CARTESIAN_POINT('Ctrl Pts',(-46.,50.4166666803226,-12.3256628518316));
#10236=CARTESIAN_POINT('Ctrl Pts',(-39.8371685740842,50.2083333469893,-23.));
#10237=CARTESIAN_POINT('Ctrl Pts',(-33.6743371481684,50.0000000136559,-33.6743371481684));
#10238=CARTESIAN_POINT('Ctrl Pts',(-23.,49.7916666803226,-39.8371685740842));
#10239=CARTESIAN_POINT('Ctrl Pts',(-12.3256628518317,49.5833333469893,-46.));
#10240=CARTESIAN_POINT('Ctrl Pts',(-2.81668763803891E-15,49.3750000136559,
-46.));
#10241=CARTESIAN_POINT('Ctrl Pts',(12.3256628518316,49.1666666803226,-46.));
#10242=CARTESIAN_POINT('Ctrl Pts',(23.,48.9583333469893,-39.8371685740842));
#10243=CARTESIAN_POINT('Ctrl Pts',(33.6743371481683,48.7500000136559,-33.6743371481684));
#10244=CARTESIAN_POINT('Ctrl Pts',(39.8371685740842,48.5416666803226,-23.));
#10245=CARTESIAN_POINT('Ctrl Pts',(46.,48.3333333469893,-12.3256628518317));
#10246=CARTESIAN_POINT('Ctrl Pts',(46.,48.1250000136559,-5.63337527607782E-15));
#10247=CARTESIAN_POINT('Ctrl Pts',(46.,47.9166666803226,12.3256628518316));
#10248=CARTESIAN_POINT('Ctrl Pts',(39.8371685740842,47.7083333469893,23.));
#10249=CARTESIAN_POINT('Ctrl Pts',(33.6743371481684,47.5000000136559,33.6743371481683));
#10250=CARTESIAN_POINT('Ctrl Pts',(23.,47.2916666803226,39.8371685740842));
#10251=CARTESIAN_POINT('Ctrl Pts',(12.3256628518317,47.0833333469893,46.));
#10252=CARTESIAN_POINT('Ctrl Pts',(8.45006291411674E-15,46.8750000136559,
46.));
#10253=CARTESIAN_POINT('Ctrl Pts',(-12.3256628518316,46.6666666803226,46.));
#10254=CARTESIAN_POINT('Ctrl Pts',(-23.,46.4583333469893,39.8371685740842));
#10255=CARTESIAN_POINT('Ctrl Pts',(-33.6743371481683,46.2500000136559,33.6743371481684));
#10256=CARTESIAN_POINT('Ctrl Pts',(-39.8371685740842,46.0416666803226,23.));
#10257=CARTESIAN_POINT('Ctrl Pts',(-46.,45.8333333469892,12.3256628518317));
#10258=CARTESIAN_POINT('Ctrl Pts',(-46.,45.6250000136559,0.));
#10259=CARTESIAN_POINT('Ctrl Pts',(-46.,45.4166666803226,-12.3256628518316));
#10260=CARTESIAN_POINT('Ctrl Pts',(-39.8371685740842,45.2083333469893,-23.));
#10261=CARTESIAN_POINT('Ctrl Pts',(-33.6743371481684,45.0000000136559,-33.6743371481684));
#10262=CARTESIAN_POINT('Ctrl Pts',(-23.,44.7916666803226,-39.8371685740842));
#10263=CARTESIAN_POINT('Ctrl Pts',(-12.3256628518317,44.5833333469893,-46.));
#10264=CARTESIAN_POINT('Ctrl Pts',(-2.81668763803891E-15,44.3750000136559,
-46.));
#10265=CARTESIAN_POINT('Ctrl Pts',(12.3256628518316,44.1666666803226,-46.));
#10266=CARTESIAN_POINT('Ctrl Pts',(23.,43.9583333469893,-39.8371685740842));
#10267=CARTESIAN_POINT('Ctrl Pts',(33.6743371481683,43.7500000136559,-33.6743371481684));
#10268=CARTESIAN_POINT('Ctrl Pts',(39.8371685740842,43.5416666803226,-23.));
#10269=CARTESIAN_POINT('Ctrl Pts',(46.,43.3333333469893,-12.3256628518317));
#10270=CARTESIAN_POINT('Ctrl Pts',(46.,43.1250000136559,-5.63337527607782E-15));
#10271=CARTESIAN_POINT('Ctrl Pts',(46.,42.9166666803226,12.3256628518316));
#10272=CARTESIAN_POINT('Ctrl Pts',(39.8371685740842,42.7083333469893,23.));
#10273=CARTESIAN_POINT('Ctrl Pts',(33.6743371481684,42.5000000136559,33.6743371481683));
#10274=CARTESIAN_POINT('Ctrl Pts',(23.,42.2916666803226,39.8371685740842));
#10275=CARTESIAN_POINT('Ctrl Pts',(12.3256628518317,42.0833333469893,46.));
#10276=CARTESIAN_POINT('Ctrl Pts',(8.45006291411674E-15,41.8750000136559,
46.));
#10277=CARTESIAN_POINT('Ctrl Pts',(-12.3256628518316,41.6666666803226,46.));
#10278=CARTESIAN_POINT('Ctrl Pts',(-23.,41.4583333469893,39.8371685740842));
#10279=CARTESIAN_POINT('Ctrl Pts',(-33.6743371481683,41.2500000136559,33.6743371481684));
#10280=CARTESIAN_POINT('Ctrl Pts',(-39.8371685740842,41.0416666803226,23.));
#10281=CARTESIAN_POINT('Ctrl Pts',(-46.,40.8333333469893,12.3256628518317));
#10282=CARTESIAN_POINT('Ctrl Pts',(-46.,40.6250000136559,0.));
#10283=CARTESIAN_POINT('Ctrl Pts',(-46.,40.4166666803226,-12.3256628518316));
#10284=CARTESIAN_POINT('Ctrl Pts',(-39.8371685740842,40.2083333469893,-23.));
#10285=CARTESIAN_POINT('Ctrl Pts',(-33.6743371481684,40.0000000136559,-33.6743371481684));
#10286=CARTESIAN_POINT('Ctrl Pts',(-23.,39.7916666803226,-39.8371685740842));
#10287=CARTESIAN_POINT('Ctrl Pts',(-12.3256628518317,39.5833333469893,-46.));
#10288=CARTESIAN_POINT('Ctrl Pts',(-2.81668763803891E-15,39.3750000136559,
-46.));
#10289=CARTESIAN_POINT('Ctrl Pts',(12.3256628518316,39.1666666803226,-46.));
#10290=CARTESIAN_POINT('Ctrl Pts',(23.,38.9583333469893,-39.8371685740842));
#10291=CARTESIAN_POINT('Ctrl Pts',(33.6743371481683,38.7500000136559,-33.6743371481684));
#10292=CARTESIAN_POINT('Ctrl Pts',(39.8371685740842,38.5416666803226,-23.));
#10293=CARTESIAN_POINT('Ctrl Pts',(46.,38.3333333469893,-12.3256628518317));
#10294=CARTESIAN_POINT('Ctrl Pts',(46.,38.1250000136559,-5.63337527607782E-15));
#10295=CARTESIAN_POINT('Ctrl Pts',(46.,37.9166666803226,12.3256628518316));
#10296=CARTESIAN_POINT('Ctrl Pts',(39.8371685740842,37.7083333469893,23.));
#10297=CARTESIAN_POINT('Ctrl Pts',(33.6743371481684,37.5000000136559,33.6743371481683));
#10298=CARTESIAN_POINT('Ctrl Pts',(23.,37.2916666803226,39.8371685740842));
#10299=CARTESIAN_POINT('Ctrl Pts',(12.3256628518317,37.0833333469893,46.));
#10300=CARTESIAN_POINT('Ctrl Pts',(8.45006291411674E-15,36.8750000136559,
46.));
#10301=CARTESIAN_POINT('Ctrl Pts',(-12.3256628518316,36.6666666803226,46.));
#10302=CARTESIAN_POINT('Ctrl Pts',(-23.,36.4583333469893,39.8371685740842));
#10303=CARTESIAN_POINT('Ctrl Pts',(-33.6743371481683,36.2500000136559,33.6743371481684));
#10304=CARTESIAN_POINT('Ctrl Pts',(-39.8371685740842,36.0416666803226,23.));
#10305=CARTESIAN_POINT('Ctrl Pts',(-46.,35.8333333469893,12.3256628518317));
#10306=CARTESIAN_POINT('Ctrl Pts',(-46.,35.6250000136559,0.));
#10307=CARTESIAN_POINT('Ctrl Pts',(-46.,35.4166666803226,-12.3256628518316));
#10308=CARTESIAN_POINT('Ctrl Pts',(-39.8371685740842,35.2083333469893,-23.));
#10309=CARTESIAN_POINT('Ctrl Pts',(-33.6743371481684,35.0000000136559,-33.6743371481684));
#10310=CARTESIAN_POINT('Ctrl Pts',(-23.,34.7916666803226,-39.8371685740842));
#10311=CARTESIAN_POINT('Ctrl Pts',(-12.3256628518317,34.5833333469893,-46.));
#10312=CARTESIAN_POINT('Ctrl Pts',(-2.81668763803891E-15,34.3750000136559,
-46.));
#10313=CARTESIAN_POINT('Ctrl Pts',(12.3256628518316,34.1666666803226,-46.));
#10314=CARTESIAN_POINT('Ctrl Pts',(23.,33.9583333469893,-39.8371685740842));
#10315=CARTESIAN_POINT('Ctrl Pts',(33.6743371481683,33.7500000136559,-33.6743371481684));
#10316=CARTESIAN_POINT('Ctrl Pts',(39.8371685740842,33.5416666803226,-23.));
#10317=CARTESIAN_POINT('Ctrl Pts',(46.,33.3333333469893,-12.3256628518317));
#10318=CARTESIAN_POINT('Ctrl Pts',(46.,33.1250000136559,-5.63337527607782E-15));
#10319=CARTESIAN_POINT('Ctrl Pts',(46.,32.9166666803226,12.3256628518316));
#10320=CARTESIAN_POINT('Ctrl Pts',(39.8371685740842,32.7083333469893,23.));
#10321=CARTESIAN_POINT('Ctrl Pts',(33.6743371481684,32.5000000136559,33.6743371481683));
#10322=CARTESIAN_POINT('Ctrl Pts',(23.,32.2916666803226,39.8371685740842));
#10323=CARTESIAN_POINT('Ctrl Pts',(12.3256628518317,32.0833333469893,46.));
#10324=CARTESIAN_POINT('Ctrl Pts',(8.45006291411674E-15,31.8750000136559,
46.));
#10325=CARTESIAN_POINT('Ctrl Pts',(-12.3256628518316,31.6666666803226,46.));
#10326=CARTESIAN_POINT('Ctrl Pts',(-23.,31.4583333469893,39.8371685740842));
#10327=CARTESIAN_POINT('Ctrl Pts',(-33.6743371481683,31.2500000136559,33.6743371481684));
#10328=CARTESIAN_POINT('Ctrl Pts',(-39.8371685740842,31.0416666803226,23.));
#10329=CARTESIAN_POINT('Ctrl Pts',(-46.,30.8333333469893,12.3256628518317));
#10330=CARTESIAN_POINT('Ctrl Pts',(-46.,30.6250000136559,0.));
#10331=CARTESIAN_POINT('Ctrl Pts',(-46.,30.4166666803226,-12.3256628518316));
#10332=CARTESIAN_POINT('Ctrl Pts',(-39.8371685740842,30.2083333469893,-23.));
#10333=CARTESIAN_POINT('Ctrl Pts',(-33.6743371481684,30.0000000136559,-33.6743371481684));
#10334=CARTESIAN_POINT('Ctrl Pts',(-23.,29.7916666803226,-39.8371685740842));
#10335=CARTESIAN_POINT('Ctrl Pts',(-12.3256628518317,29.5833333469893,-46.));
#10336=CARTESIAN_POINT('Ctrl Pts',(-2.81668763803891E-15,29.3750000136559,
-46.));
#10337=CARTESIAN_POINT('Ctrl Pts',(12.3256628518316,29.1666666803226,-46.));
#10338=CARTESIAN_POINT('Ctrl Pts',(23.,28.9583333469893,-39.8371685740842));
#10339=CARTESIAN_POINT('Ctrl Pts',(33.6743371481683,28.7500000136559,-33.6743371481684));
#10340=CARTESIAN_POINT('Ctrl Pts',(39.8371685740842,28.5416666803226,-23.));
#10341=CARTESIAN_POINT('Ctrl Pts',(46.,28.3333333469893,-12.3256628518317));
#10342=CARTESIAN_POINT('Ctrl Pts',(46.,28.1250000136559,-5.63337527607782E-15));
#10343=CARTESIAN_POINT('Ctrl Pts',(46.,27.9166666803226,12.3256628518316));
#10344=CARTESIAN_POINT('Ctrl Pts',(39.8371685740842,27.7083333469893,23.));
#10345=CARTESIAN_POINT('Ctrl Pts',(33.6743371481684,27.5000000136559,33.6743371481683));
#10346=CARTESIAN_POINT('Ctrl Pts',(23.,27.2916666803226,39.8371685740842));
#10347=CARTESIAN_POINT('Ctrl Pts',(12.3256628518317,27.0833333469893,46.));
#10348=CARTESIAN_POINT('Ctrl Pts',(8.45006291411674E-15,26.8750000136559,
46.));
#10349=CARTESIAN_POINT('Ctrl Pts',(-12.3256628518316,26.6666666803226,46.));
#10350=CARTESIAN_POINT('Ctrl Pts',(-23.,26.4583333469893,39.8371685740842));
#10351=CARTESIAN_POINT('Ctrl Pts',(-33.6743371481683,26.2500000136559,33.6743371481684));
#10352=CARTESIAN_POINT('Ctrl Pts',(-39.8371685740842,26.0416666803226,23.));
#10353=CARTESIAN_POINT('Ctrl Pts',(-46.,25.8333333469893,12.3256628518317));
#10354=CARTESIAN_POINT('Ctrl Pts',(-46.,25.6250000136559,0.));
#10355=CARTESIAN_POINT('Ctrl Pts',(-48.706329375,57.187500006828,-1.8898197019151E-14));
#10356=CARTESIAN_POINT('Ctrl Pts',(-48.706329375,56.9791666734946,-13.0508216223155));
#10357=CARTESIAN_POINT('Ctrl Pts',(-42.1809185638422,56.7708333401613,-24.3531646875));
#10358=CARTESIAN_POINT('Ctrl Pts',(-35.6555077526845,56.562500006828,-35.6555077526845));
#10359=CARTESIAN_POINT('Ctrl Pts',(-24.3531646875,56.3541666734946,-42.1809185638423));
#10360=CARTESIAN_POINT('Ctrl Pts',(-13.0508216223155,56.1458333401613,-48.706329375));
#10361=CARTESIAN_POINT('Ctrl Pts',(1.59157945007855E-14,55.937500006828,
-48.706329375));
#10362=CARTESIAN_POINT('Ctrl Pts',(13.0508216223155,55.7291666734946,-48.706329375));
#10363=CARTESIAN_POINT('Ctrl Pts',(24.3531646875,55.5208333401613,-42.1809185638422));
#10364=CARTESIAN_POINT('Ctrl Pts',(35.6555077526845,55.312500006828,-35.6555077526845));
#10365=CARTESIAN_POINT('Ctrl Pts',(42.1809185638422,55.1041666734946,-24.3531646875));
#10366=CARTESIAN_POINT('Ctrl Pts',(48.706329375,54.8958333401613,-13.0508216223155));
#10367=CARTESIAN_POINT('Ctrl Pts',(48.706329375,54.687500006828,1.293339198242E-14));
#10368=CARTESIAN_POINT('Ctrl Pts',(48.706329375,54.4791666734946,13.0508216223155));
#10369=CARTESIAN_POINT('Ctrl Pts',(42.1809185638422,54.2708333401613,24.3531646875));
#10370=CARTESIAN_POINT('Ctrl Pts',(35.6555077526845,54.062500006828,35.6555077526845));
#10371=CARTESIAN_POINT('Ctrl Pts',(24.3531646875,53.8541666734946,42.1809185638422));
#10372=CARTESIAN_POINT('Ctrl Pts',(13.0508216223155,53.6458333401613,48.706329375));
#10373=CARTESIAN_POINT('Ctrl Pts',(-9.95098946405443E-15,53.437500006828,
48.706329375));
#10374=CARTESIAN_POINT('Ctrl Pts',(-13.0508216223155,53.2291666734946,48.706329375));
#10375=CARTESIAN_POINT('Ctrl Pts',(-24.3531646875,53.0208333401613,42.1809185638423));
#10376=CARTESIAN_POINT('Ctrl Pts',(-35.6555077526845,52.812500006828,35.6555077526845));
#10377=CARTESIAN_POINT('Ctrl Pts',(-42.1809185638422,52.6041666734946,24.3531646875));
#10378=CARTESIAN_POINT('Ctrl Pts',(-48.706329375,52.3958333401613,13.0508216223155));
#10379=CARTESIAN_POINT('Ctrl Pts',(-48.706329375,52.187500006828,-1.8898197019151E-14));
#10380=CARTESIAN_POINT('Ctrl Pts',(-48.706329375,51.9791666734946,-13.0508216223155));
#10381=CARTESIAN_POINT('Ctrl Pts',(-42.1809185638422,51.7708333401613,-24.3531646875));
#10382=CARTESIAN_POINT('Ctrl Pts',(-35.6555077526845,51.562500006828,-35.6555077526845));
#10383=CARTESIAN_POINT('Ctrl Pts',(-24.3531646875,51.3541666734946,-42.1809185638423));
#10384=CARTESIAN_POINT('Ctrl Pts',(-13.0508216223155,51.1458333401613,-48.706329375));
#10385=CARTESIAN_POINT('Ctrl Pts',(1.59157945007855E-14,50.937500006828,
-48.706329375));
#10386=CARTESIAN_POINT('Ctrl Pts',(13.0508216223155,50.7291666734946,-48.706329375));
#10387=CARTESIAN_POINT('Ctrl Pts',(24.3531646875,50.5208333401613,-42.1809185638422));
#10388=CARTESIAN_POINT('Ctrl Pts',(35.6555077526845,50.312500006828,-35.6555077526845));
#10389=CARTESIAN_POINT('Ctrl Pts',(42.1809185638422,50.1041666734946,-24.3531646875));
#10390=CARTESIAN_POINT('Ctrl Pts',(48.706329375,49.8958333401613,-13.0508216223155));
#10391=CARTESIAN_POINT('Ctrl Pts',(48.706329375,49.687500006828,1.293339198242E-14));
#10392=CARTESIAN_POINT('Ctrl Pts',(48.706329375,49.4791666734946,13.0508216223155));
#10393=CARTESIAN_POINT('Ctrl Pts',(42.1809185638422,49.2708333401613,24.3531646875));
#10394=CARTESIAN_POINT('Ctrl Pts',(35.6555077526845,49.062500006828,35.6555077526845));
#10395=CARTESIAN_POINT('Ctrl Pts',(24.3531646875,48.8541666734946,42.1809185638422));
#10396=CARTESIAN_POINT('Ctrl Pts',(13.0508216223155,48.6458333401613,48.706329375));
#10397=CARTESIAN_POINT('Ctrl Pts',(-9.95098946405443E-15,48.437500006828,
48.706329375));
#10398=CARTESIAN_POINT('Ctrl Pts',(-13.0508216223155,48.2291666734946,48.706329375));
#10399=CARTESIAN_POINT('Ctrl Pts',(-24.3531646875,48.0208333401613,42.1809185638423));
#10400=CARTESIAN_POINT('Ctrl Pts',(-35.6555077526845,47.812500006828,35.6555077526845));
#10401=CARTESIAN_POINT('Ctrl Pts',(-42.1809185638422,47.6041666734946,24.3531646875));
#10402=CARTESIAN_POINT('Ctrl Pts',(-48.706329375,47.3958333401613,13.0508216223155));
#10403=CARTESIAN_POINT('Ctrl Pts',(-48.706329375,47.187500006828,-1.8898197019151E-14));
#10404=CARTESIAN_POINT('Ctrl Pts',(-48.706329375,46.9791666734946,-13.0508216223155));
#10405=CARTESIAN_POINT('Ctrl Pts',(-42.1809185638422,46.7708333401613,-24.3531646875));
#10406=CARTESIAN_POINT('Ctrl Pts',(-35.6555077526845,46.562500006828,-35.6555077526845));
#10407=CARTESIAN_POINT('Ctrl Pts',(-24.3531646875,46.3541666734946,-42.1809185638423));
#10408=CARTESIAN_POINT('Ctrl Pts',(-13.0508216223155,46.1458333401613,-48.706329375));
#10409=CARTESIAN_POINT('Ctrl Pts',(1.59157945007855E-14,45.937500006828,
-48.706329375));
#10410=CARTESIAN_POINT('Ctrl Pts',(13.0508216223155,45.7291666734946,-48.706329375));
#10411=CARTESIAN_POINT('Ctrl Pts',(24.3531646875,45.5208333401613,-42.1809185638422));
#10412=CARTESIAN_POINT('Ctrl Pts',(35.6555077526845,45.312500006828,-35.6555077526845));
#10413=CARTESIAN_POINT('Ctrl Pts',(42.1809185638422,45.1041666734946,-24.3531646875));
#10414=CARTESIAN_POINT('Ctrl Pts',(48.706329375,44.8958333401613,-13.0508216223155));
#10415=CARTESIAN_POINT('Ctrl Pts',(48.706329375,44.687500006828,1.293339198242E-14));
#10416=CARTESIAN_POINT('Ctrl Pts',(48.706329375,44.4791666734946,13.0508216223155));
#10417=CARTESIAN_POINT('Ctrl Pts',(42.1809185638422,44.2708333401613,24.3531646875));
#10418=CARTESIAN_POINT('Ctrl Pts',(35.6555077526845,44.062500006828,35.6555077526845));
#10419=CARTESIAN_POINT('Ctrl Pts',(24.3531646875,43.8541666734946,42.1809185638422));
#10420=CARTESIAN_POINT('Ctrl Pts',(13.0508216223155,43.6458333401613,48.706329375));
#10421=CARTESIAN_POINT('Ctrl Pts',(-9.95098946405443E-15,43.437500006828,
48.706329375));
#10422=CARTESIAN_POINT('Ctrl Pts',(-13.0508216223155,43.2291666734946,48.706329375));
#10423=CARTESIAN_POINT('Ctrl Pts',(-24.3531646875,43.0208333401613,42.1809185638423));
#10424=CARTESIAN_POINT('Ctrl Pts',(-35.6555077526845,42.812500006828,35.6555077526845));
#10425=CARTESIAN_POINT('Ctrl Pts',(-42.1809185638422,42.6041666734946,24.3531646875));
#10426=CARTESIAN_POINT('Ctrl Pts',(-48.706329375,42.3958333401613,13.0508216223155));
#10427=CARTESIAN_POINT('Ctrl Pts',(-48.706329375,42.187500006828,-1.8898197019151E-14));
#10428=CARTESIAN_POINT('Ctrl Pts',(-48.706329375,41.9791666734946,-13.0508216223155));
#10429=CARTESIAN_POINT('Ctrl Pts',(-42.1809185638422,41.7708333401613,-24.3531646875));
#10430=CARTESIAN_POINT('Ctrl Pts',(-35.6555077526845,41.562500006828,-35.6555077526845));
#10431=CARTESIAN_POINT('Ctrl Pts',(-24.3531646875,41.3541666734946,-42.1809185638423));
#10432=CARTESIAN_POINT('Ctrl Pts',(-13.0508216223155,41.1458333401613,-48.706329375));
#10433=CARTESIAN_POINT('Ctrl Pts',(1.59157945007855E-14,40.937500006828,
-48.706329375));
#10434=CARTESIAN_POINT('Ctrl Pts',(13.0508216223155,40.7291666734946,-48.706329375));
#10435=CARTESIAN_POINT('Ctrl Pts',(24.3531646875,40.5208333401613,-42.1809185638422));
#10436=CARTESIAN_POINT('Ctrl Pts',(35.6555077526845,40.312500006828,-35.6555077526845));
#10437=CARTESIAN_POINT('Ctrl Pts',(42.1809185638422,40.1041666734946,-24.3531646875));
#10438=CARTESIAN_POINT('Ctrl Pts',(48.706329375,39.8958333401613,-13.0508216223155));
#10439=CARTESIAN_POINT('Ctrl Pts',(48.706329375,39.687500006828,1.293339198242E-14));
#10440=CARTESIAN_POINT('Ctrl Pts',(48.706329375,39.4791666734946,13.0508216223155));
#10441=CARTESIAN_POINT('Ctrl Pts',(42.1809185638422,39.2708333401613,24.3531646875));
#10442=CARTESIAN_POINT('Ctrl Pts',(35.6555077526845,39.062500006828,35.6555077526845));
#10443=CARTESIAN_POINT('Ctrl Pts',(24.3531646875,38.8541666734946,42.1809185638422));
#10444=CARTESIAN_POINT('Ctrl Pts',(13.0508216223155,38.6458333401613,48.706329375));
#10445=CARTESIAN_POINT('Ctrl Pts',(-9.95098946405443E-15,38.437500006828,
48.706329375));
#10446=CARTESIAN_POINT('Ctrl Pts',(-13.0508216223155,38.2291666734946,48.706329375));
#10447=CARTESIAN_POINT('Ctrl Pts',(-24.3531646875,38.0208333401613,42.1809185638423));
#10448=CARTESIAN_POINT('Ctrl Pts',(-35.6555077526845,37.812500006828,35.6555077526845));
#10449=CARTESIAN_POINT('Ctrl Pts',(-42.1809185638422,37.6041666734946,24.3531646875));
#10450=CARTESIAN_POINT('Ctrl Pts',(-48.706329375,37.3958333401613,13.0508216223155));
#10451=CARTESIAN_POINT('Ctrl Pts',(-48.706329375,37.187500006828,-1.8898197019151E-14));
#10452=CARTESIAN_POINT('Ctrl Pts',(-48.706329375,36.9791666734946,-13.0508216223155));
#10453=CARTESIAN_POINT('Ctrl Pts',(-42.1809185638422,36.7708333401613,-24.3531646875));
#10454=CARTESIAN_POINT('Ctrl Pts',(-35.6555077526845,36.562500006828,-35.6555077526845));
#10455=CARTESIAN_POINT('Ctrl Pts',(-24.3531646875,36.3541666734946,-42.1809185638423));
#10456=CARTESIAN_POINT('Ctrl Pts',(-13.0508216223155,36.1458333401613,-48.706329375));
#10457=CARTESIAN_POINT('Ctrl Pts',(1.59157945007855E-14,35.937500006828,
-48.706329375));
#10458=CARTESIAN_POINT('Ctrl Pts',(13.0508216223155,35.7291666734946,-48.706329375));
#10459=CARTESIAN_POINT('Ctrl Pts',(24.3531646875,35.5208333401613,-42.1809185638422));
#10460=CARTESIAN_POINT('Ctrl Pts',(35.6555077526845,35.312500006828,-35.6555077526845));
#10461=CARTESIAN_POINT('Ctrl Pts',(42.1809185638422,35.1041666734946,-24.3531646875));
#10462=CARTESIAN_POINT('Ctrl Pts',(48.706329375,34.8958333401613,-13.0508216223155));
#10463=CARTESIAN_POINT('Ctrl Pts',(48.706329375,34.687500006828,1.293339198242E-14));
#10464=CARTESIAN_POINT('Ctrl Pts',(48.706329375,34.4791666734946,13.0508216223155));
#10465=CARTESIAN_POINT('Ctrl Pts',(42.1809185638422,34.2708333401613,24.3531646875));
#10466=CARTESIAN_POINT('Ctrl Pts',(35.6555077526845,34.062500006828,35.6555077526845));
#10467=CARTESIAN_POINT('Ctrl Pts',(24.3531646875,33.8541666734946,42.1809185638422));
#10468=CARTESIAN_POINT('Ctrl Pts',(13.0508216223155,33.6458333401613,48.706329375));
#10469=CARTESIAN_POINT('Ctrl Pts',(-9.95098946405443E-15,33.437500006828,
48.706329375));
#10470=CARTESIAN_POINT('Ctrl Pts',(-13.0508216223155,33.2291666734946,48.706329375));
#10471=CARTESIAN_POINT('Ctrl Pts',(-24.3531646875,33.0208333401613,42.1809185638423));
#10472=CARTESIAN_POINT('Ctrl Pts',(-35.6555077526845,32.812500006828,35.6555077526845));
#10473=CARTESIAN_POINT('Ctrl Pts',(-42.1809185638422,32.6041666734946,24.3531646875));
#10474=CARTESIAN_POINT('Ctrl Pts',(-48.706329375,32.3958333401613,13.0508216223155));
#10475=CARTESIAN_POINT('Ctrl Pts',(-48.706329375,32.187500006828,-1.8898197019151E-14));
#10476=CARTESIAN_POINT('Ctrl Pts',(-48.706329375,31.9791666734946,-13.0508216223155));
#10477=CARTESIAN_POINT('Ctrl Pts',(-42.1809185638422,31.7708333401613,-24.3531646875));
#10478=CARTESIAN_POINT('Ctrl Pts',(-35.6555077526845,31.562500006828,-35.6555077526845));
#10479=CARTESIAN_POINT('Ctrl Pts',(-24.3531646875,31.3541666734946,-42.1809185638423));
#10480=CARTESIAN_POINT('Ctrl Pts',(-13.0508216223155,31.1458333401613,-48.706329375));
#10481=CARTESIAN_POINT('Ctrl Pts',(1.59157945007855E-14,30.937500006828,
-48.706329375));
#10482=CARTESIAN_POINT('Ctrl Pts',(13.0508216223155,30.7291666734946,-48.706329375));
#10483=CARTESIAN_POINT('Ctrl Pts',(24.3531646875,30.5208333401613,-42.1809185638422));
#10484=CARTESIAN_POINT('Ctrl Pts',(35.6555077526845,30.312500006828,-35.6555077526845));
#10485=CARTESIAN_POINT('Ctrl Pts',(42.1809185638422,30.1041666734946,-24.3531646875));
#10486=CARTESIAN_POINT('Ctrl Pts',(48.706329375,29.8958333401613,-13.0508216223155));
#10487=CARTESIAN_POINT('Ctrl Pts',(48.706329375,29.687500006828,1.293339198242E-14));
#10488=CARTESIAN_POINT('Ctrl Pts',(48.706329375,29.4791666734946,13.0508216223155));
#10489=CARTESIAN_POINT('Ctrl Pts',(42.1809185638422,29.2708333401613,24.3531646875));
#10490=CARTESIAN_POINT('Ctrl Pts',(35.6555077526845,29.062500006828,35.6555077526845));
#10491=CARTESIAN_POINT('Ctrl Pts',(24.3531646875,28.8541666734946,42.1809185638422));
#10492=CARTESIAN_POINT('Ctrl Pts',(13.0508216223155,28.6458333401613,48.706329375));
#10493=CARTESIAN_POINT('Ctrl Pts',(-9.95098946405443E-15,28.437500006828,
48.706329375));
#10494=CARTESIAN_POINT('Ctrl Pts',(-13.0508216223155,28.2291666734946,48.706329375));
#10495=CARTESIAN_POINT('Ctrl Pts',(-24.3531646875,28.0208333401613,42.1809185638423));
#10496=CARTESIAN_POINT('Ctrl Pts',(-35.6555077526845,27.812500006828,35.6555077526845));
#10497=CARTESIAN_POINT('Ctrl Pts',(-42.1809185638422,27.6041666734946,24.3531646875));
#10498=CARTESIAN_POINT('Ctrl Pts',(-48.706329375,27.3958333401613,13.0508216223155));
#10499=CARTESIAN_POINT('Ctrl Pts',(-48.706329375,27.187500006828,-1.8898197019151E-14));
#10500=CARTESIAN_POINT('',(-45.7957082162897,35.5508791552084,-4.33048599679673));
#10501=CARTESIAN_POINT('',(-3.42983911135813,34.4335524565479,-45.8719544348199));
#10502=CARTESIAN_POINT('Ctrl Pts',(-45.7957082162897,35.5508791552084,-4.33048599679673));
#10503=CARTESIAN_POINT('Ctrl Pts',(-44.8515840435634,35.3778446993657,-14.3147776366027));
#10504=CARTESIAN_POINT('Ctrl Pts',(-39.8371685740842,35.2083333469893,-23.));
#10505=CARTESIAN_POINT('Ctrl Pts',(-33.6743371481684,35.0000000136559,-33.6743371481684));
#10506=CARTESIAN_POINT('Ctrl Pts',(-23.,34.7916666803226,-39.8371685740842));
#10507=CARTESIAN_POINT('Ctrl Pts',(-13.903887812949,34.6141359029078,-45.0888113938571));
#10508=CARTESIAN_POINT('Ctrl Pts',(-3.42983911135813,34.4335524565479,-45.8719544348199));
#10509=CARTESIAN_POINT('',(-48.5134353784344,37.1175463684955,-4.33048599679682));
#10510=CARTESIAN_POINT('Ctrl Pts',(-45.7957082162897,35.5508791552084,-4.33048599679673));
#10511=CARTESIAN_POINT('Ctrl Pts',(-46.027322302781,35.6843839384496,-4.33048599679679));
#10512=CARTESIAN_POINT('Ctrl Pts',(-46.4905476657728,35.9513983799647,-4.33048599679657));
#10513=CARTESIAN_POINT('Ctrl Pts',(-46.9537676533565,36.2184221466352,-4.33048599679682));
#10514=CARTESIAN_POINT('Ctrl Pts',(-47.6280672732221,36.6071316973962,-4.33048599679682));
#10515=CARTESIAN_POINT('Ctrl Pts',(-48.0707534890442,36.8623352807796,-4.33048599679682));
#10516=CARTESIAN_POINT('Ctrl Pts',(-48.5134353784344,37.1175463684955,-4.33048599679682));
#10517=CARTESIAN_POINT('',(-4.2120577778781,36.0055185535964,-48.5238610423965));
#10518=CARTESIAN_POINT('Ctrl Pts',(-48.5134353784344,37.1175463684955,-4.33048599679682));
#10519=CARTESIAN_POINT('Ctrl Pts',(-47.5573898704235,36.9424850907232,-15.0408432190651));
#10520=CARTESIAN_POINT('Ctrl Pts',(-42.1809185638422,36.7708333401613,-24.3531646875));
#10521=CARTESIAN_POINT('Ctrl Pts',(-35.6555077526845,36.562500006828,-35.6555077526845));
#10522=CARTESIAN_POINT('Ctrl Pts',(-24.3531646875,36.3541666734946,-42.1809185638423));
#10523=CARTESIAN_POINT('Ctrl Pts',(-14.9868402884059,36.1815195000819,-47.5885684769766));
#10524=CARTESIAN_POINT('Ctrl Pts',(-4.2120577778781,36.0055185535964,-48.5238610423965));
#10525=CARTESIAN_POINT('Ctrl Pts',(-4.21205777787798,36.0055185535964,-48.5238610423965));
#10526=CARTESIAN_POINT('Ctrl Pts',(-4.14747432921768,35.7400881602412,-48.0687061610727));
#10527=CARTESIAN_POINT('Ctrl Pts',(-4.05341057734826,35.4727756853994,-47.6137074546591));
#10528=CARTESIAN_POINT('Ctrl Pts',(-3.79876998734544,34.948351505957,-46.7286766926143));
#10529=CARTESIAN_POINT('Ctrl Pts',(-3.63547301092605,34.6853692057132,-46.2887605423145));
#10530=CARTESIAN_POINT('Ctrl Pts',(-3.42983911135814,34.4335524565479,-45.87195443482));
#10531=CARTESIAN_POINT('Ctrl Pts',(-46.,55.6250000136559,0.));
#10532=CARTESIAN_POINT('Ctrl Pts',(-46.,55.4166666803226,-12.3256628518316));
#10533=CARTESIAN_POINT('Ctrl Pts',(-39.8371685740842,55.2083333469893,-23.));
#10534=CARTESIAN_POINT('Ctrl Pts',(-33.6743371481684,55.0000000136559,-33.6743371481684));
#10535=CARTESIAN_POINT('Ctrl Pts',(-23.,54.7916666803226,-39.8371685740842));
#10536=CARTESIAN_POINT('Ctrl Pts',(-12.3256628518317,54.5833333469893,-46.));
#10537=CARTESIAN_POINT('Ctrl Pts',(-2.81668763803891E-15,54.3750000136559,
-46.));
#10538=CARTESIAN_POINT('Ctrl Pts',(12.3256628518316,54.1666666803226,-46.));
#10539=CARTESIAN_POINT('Ctrl Pts',(23.,53.9583333469893,-39.8371685740842));
#10540=CARTESIAN_POINT('Ctrl Pts',(33.6743371481683,53.7500000136559,-33.6743371481684));
#10541=CARTESIAN_POINT('Ctrl Pts',(39.8371685740842,53.5416666803226,-23.));
#10542=CARTESIAN_POINT('Ctrl Pts',(46.,53.3333333469893,-12.3256628518317));
#10543=CARTESIAN_POINT('Ctrl Pts',(46.,53.1250000136559,-5.63337527607782E-15));
#10544=CARTESIAN_POINT('Ctrl Pts',(46.,52.9166666803226,12.3256628518316));
#10545=CARTESIAN_POINT('Ctrl Pts',(39.8371685740842,52.7083333469893,23.));
#10546=CARTESIAN_POINT('Ctrl Pts',(33.6743371481684,52.5000000136559,33.6743371481683));
#10547=CARTESIAN_POINT('Ctrl Pts',(23.,52.2916666803226,39.8371685740842));
#10548=CARTESIAN_POINT('Ctrl Pts',(12.3256628518317,52.0833333469893,46.));
#10549=CARTESIAN_POINT('Ctrl Pts',(8.45006291411674E-15,51.8750000136559,
46.));
#10550=CARTESIAN_POINT('Ctrl Pts',(-12.3256628518316,51.6666666803226,46.));
#10551=CARTESIAN_POINT('Ctrl Pts',(-23.,51.4583333469893,39.8371685740842));
#10552=CARTESIAN_POINT('Ctrl Pts',(-33.6743371481683,51.2500000136559,33.6743371481684));
#10553=CARTESIAN_POINT('Ctrl Pts',(-39.8371685740842,51.0416666803226,23.));
#10554=CARTESIAN_POINT('Ctrl Pts',(-46.,50.8333333469893,12.3256628518317));
#10555=CARTESIAN_POINT('Ctrl Pts',(-46.,50.6250000136559,0.));
#10556=CARTESIAN_POINT('Ctrl Pts',(-46.,50.4166666803226,-12.3256628518316));
#10557=CARTESIAN_POINT('Ctrl Pts',(-39.8371685740842,50.2083333469893,-23.));
#10558=CARTESIAN_POINT('Ctrl Pts',(-33.6743371481684,50.0000000136559,-33.6743371481684));
#10559=CARTESIAN_POINT('Ctrl Pts',(-23.,49.7916666803226,-39.8371685740842));
#10560=CARTESIAN_POINT('Ctrl Pts',(-12.3256628518317,49.5833333469893,-46.));
#10561=CARTESIAN_POINT('Ctrl Pts',(-2.81668763803891E-15,49.3750000136559,
-46.));
#10562=CARTESIAN_POINT('Ctrl Pts',(12.3256628518316,49.1666666803226,-46.));
#10563=CARTESIAN_POINT('Ctrl Pts',(23.,48.9583333469893,-39.8371685740842));
#10564=CARTESIAN_POINT('Ctrl Pts',(33.6743371481683,48.7500000136559,-33.6743371481684));
#10565=CARTESIAN_POINT('Ctrl Pts',(39.8371685740842,48.5416666803226,-23.));
#10566=CARTESIAN_POINT('Ctrl Pts',(46.,48.3333333469893,-12.3256628518317));
#10567=CARTESIAN_POINT('Ctrl Pts',(46.,48.1250000136559,-5.63337527607782E-15));
#10568=CARTESIAN_POINT('Ctrl Pts',(46.,47.9166666803226,12.3256628518316));
#10569=CARTESIAN_POINT('Ctrl Pts',(39.8371685740842,47.7083333469893,23.));
#10570=CARTESIAN_POINT('Ctrl Pts',(33.6743371481684,47.5000000136559,33.6743371481683));
#10571=CARTESIAN_POINT('Ctrl Pts',(23.,47.2916666803226,39.8371685740842));
#10572=CARTESIAN_POINT('Ctrl Pts',(12.3256628518317,47.0833333469893,46.));
#10573=CARTESIAN_POINT('Ctrl Pts',(8.45006291411674E-15,46.8750000136559,
46.));
#10574=CARTESIAN_POINT('Ctrl Pts',(-12.3256628518316,46.6666666803226,46.));
#10575=CARTESIAN_POINT('Ctrl Pts',(-23.,46.4583333469893,39.8371685740842));
#10576=CARTESIAN_POINT('Ctrl Pts',(-33.6743371481683,46.2500000136559,33.6743371481684));
#10577=CARTESIAN_POINT('Ctrl Pts',(-39.8371685740842,46.0416666803226,23.));
#10578=CARTESIAN_POINT('Ctrl Pts',(-46.,45.8333333469892,12.3256628518317));
#10579=CARTESIAN_POINT('Ctrl Pts',(-46.,45.6250000136559,0.));
#10580=CARTESIAN_POINT('Ctrl Pts',(-46.,45.4166666803226,-12.3256628518316));
#10581=CARTESIAN_POINT('Ctrl Pts',(-39.8371685740842,45.2083333469893,-23.));
#10582=CARTESIAN_POINT('Ctrl Pts',(-33.6743371481684,45.0000000136559,-33.6743371481684));
#10583=CARTESIAN_POINT('Ctrl Pts',(-23.,44.7916666803226,-39.8371685740842));
#10584=CARTESIAN_POINT('Ctrl Pts',(-12.3256628518317,44.5833333469893,-46.));
#10585=CARTESIAN_POINT('Ctrl Pts',(-2.81668763803891E-15,44.3750000136559,
-46.));
#10586=CARTESIAN_POINT('Ctrl Pts',(12.3256628518316,44.1666666803226,-46.));
#10587=CARTESIAN_POINT('Ctrl Pts',(23.,43.9583333469893,-39.8371685740842));
#10588=CARTESIAN_POINT('Ctrl Pts',(33.6743371481683,43.7500000136559,-33.6743371481684));
#10589=CARTESIAN_POINT('Ctrl Pts',(39.8371685740842,43.5416666803226,-23.));
#10590=CARTESIAN_POINT('Ctrl Pts',(46.,43.3333333469893,-12.3256628518317));
#10591=CARTESIAN_POINT('Ctrl Pts',(46.,43.1250000136559,-5.63337527607782E-15));
#10592=CARTESIAN_POINT('Ctrl Pts',(46.,42.9166666803226,12.3256628518316));
#10593=CARTESIAN_POINT('Ctrl Pts',(39.8371685740842,42.7083333469893,23.));
#10594=CARTESIAN_POINT('Ctrl Pts',(33.6743371481684,42.5000000136559,33.6743371481683));
#10595=CARTESIAN_POINT('Ctrl Pts',(23.,42.2916666803226,39.8371685740842));
#10596=CARTESIAN_POINT('Ctrl Pts',(12.3256628518317,42.0833333469893,46.));
#10597=CARTESIAN_POINT('Ctrl Pts',(8.45006291411674E-15,41.8750000136559,
46.));
#10598=CARTESIAN_POINT('Ctrl Pts',(-12.3256628518316,41.6666666803226,46.));
#10599=CARTESIAN_POINT('Ctrl Pts',(-23.,41.4583333469893,39.8371685740842));
#10600=CARTESIAN_POINT('Ctrl Pts',(-33.6743371481683,41.2500000136559,33.6743371481684));
#10601=CARTESIAN_POINT('Ctrl Pts',(-39.8371685740842,41.0416666803226,23.));
#10602=CARTESIAN_POINT('Ctrl Pts',(-46.,40.8333333469893,12.3256628518317));
#10603=CARTESIAN_POINT('Ctrl Pts',(-46.,40.6250000136559,0.));
#10604=CARTESIAN_POINT('Ctrl Pts',(-46.,40.4166666803226,-12.3256628518316));
#10605=CARTESIAN_POINT('Ctrl Pts',(-39.8371685740842,40.2083333469893,-23.));
#10606=CARTESIAN_POINT('Ctrl Pts',(-33.6743371481684,40.0000000136559,-33.6743371481684));
#10607=CARTESIAN_POINT('Ctrl Pts',(-23.,39.7916666803226,-39.8371685740842));
#10608=CARTESIAN_POINT('Ctrl Pts',(-12.3256628518317,39.5833333469893,-46.));
#10609=CARTESIAN_POINT('Ctrl Pts',(-2.81668763803891E-15,39.3750000136559,
-46.));
#10610=CARTESIAN_POINT('Ctrl Pts',(12.3256628518316,39.1666666803226,-46.));
#10611=CARTESIAN_POINT('Ctrl Pts',(23.,38.9583333469893,-39.8371685740842));
#10612=CARTESIAN_POINT('Ctrl Pts',(33.6743371481683,38.7500000136559,-33.6743371481684));
#10613=CARTESIAN_POINT('Ctrl Pts',(39.8371685740842,38.5416666803226,-23.));
#10614=CARTESIAN_POINT('Ctrl Pts',(46.,38.3333333469893,-12.3256628518317));
#10615=CARTESIAN_POINT('Ctrl Pts',(46.,38.1250000136559,-5.63337527607782E-15));
#10616=CARTESIAN_POINT('Ctrl Pts',(46.,37.9166666803226,12.3256628518316));
#10617=CARTESIAN_POINT('Ctrl Pts',(39.8371685740842,37.7083333469893,23.));
#10618=CARTESIAN_POINT('Ctrl Pts',(33.6743371481684,37.5000000136559,33.6743371481683));
#10619=CARTESIAN_POINT('Ctrl Pts',(23.,37.2916666803226,39.8371685740842));
#10620=CARTESIAN_POINT('Ctrl Pts',(12.3256628518317,37.0833333469893,46.));
#10621=CARTESIAN_POINT('Ctrl Pts',(8.45006291411674E-15,36.8750000136559,
46.));
#10622=CARTESIAN_POINT('Ctrl Pts',(-12.3256628518316,36.6666666803226,46.));
#10623=CARTESIAN_POINT('Ctrl Pts',(-23.,36.4583333469893,39.8371685740842));
#10624=CARTESIAN_POINT('Ctrl Pts',(-33.6743371481683,36.2500000136559,33.6743371481684));
#10625=CARTESIAN_POINT('Ctrl Pts',(-39.8371685740842,36.0416666803226,23.));
#10626=CARTESIAN_POINT('Ctrl Pts',(-46.,35.8333333469893,12.3256628518317));
#10627=CARTESIAN_POINT('Ctrl Pts',(-46.,35.6250000136559,0.));
#10628=CARTESIAN_POINT('Ctrl Pts',(-46.,35.4166666803226,-12.3256628518316));
#10629=CARTESIAN_POINT('Ctrl Pts',(-39.8371685740842,35.2083333469893,-23.));
#10630=CARTESIAN_POINT('Ctrl Pts',(-33.6743371481684,35.0000000136559,-33.6743371481684));
#10631=CARTESIAN_POINT('Ctrl Pts',(-23.,34.7916666803226,-39.8371685740842));
#10632=CARTESIAN_POINT('Ctrl Pts',(-12.3256628518317,34.5833333469893,-46.));
#10633=CARTESIAN_POINT('Ctrl Pts',(-2.81668763803891E-15,34.3750000136559,
-46.));
#10634=CARTESIAN_POINT('Ctrl Pts',(12.3256628518316,34.1666666803226,-46.));
#10635=CARTESIAN_POINT('Ctrl Pts',(23.,33.9583333469893,-39.8371685740842));
#10636=CARTESIAN_POINT('Ctrl Pts',(33.6743371481683,33.7500000136559,-33.6743371481684));
#10637=CARTESIAN_POINT('Ctrl Pts',(39.8371685740842,33.5416666803226,-23.));
#10638=CARTESIAN_POINT('Ctrl Pts',(46.,33.3333333469893,-12.3256628518317));
#10639=CARTESIAN_POINT('Ctrl Pts',(46.,33.1250000136559,-5.63337527607782E-15));
#10640=CARTESIAN_POINT('Ctrl Pts',(46.,32.9166666803226,12.3256628518316));
#10641=CARTESIAN_POINT('Ctrl Pts',(39.8371685740842,32.7083333469893,23.));
#10642=CARTESIAN_POINT('Ctrl Pts',(33.6743371481684,32.5000000136559,33.6743371481683));
#10643=CARTESIAN_POINT('Ctrl Pts',(23.,32.2916666803226,39.8371685740842));
#10644=CARTESIAN_POINT('Ctrl Pts',(12.3256628518317,32.0833333469893,46.));
#10645=CARTESIAN_POINT('Ctrl Pts',(8.45006291411674E-15,31.8750000136559,
46.));
#10646=CARTESIAN_POINT('Ctrl Pts',(-12.3256628518316,31.6666666803226,46.));
#10647=CARTESIAN_POINT('Ctrl Pts',(-23.,31.4583333469893,39.8371685740842));
#10648=CARTESIAN_POINT('Ctrl Pts',(-33.6743371481683,31.2500000136559,33.6743371481684));
#10649=CARTESIAN_POINT('Ctrl Pts',(-39.8371685740842,31.0416666803226,23.));
#10650=CARTESIAN_POINT('Ctrl Pts',(-46.,30.8333333469893,12.3256628518317));
#10651=CARTESIAN_POINT('Ctrl Pts',(-46.,30.6250000136559,0.));
#10652=CARTESIAN_POINT('Ctrl Pts',(-46.,30.4166666803226,-12.3256628518316));
#10653=CARTESIAN_POINT('Ctrl Pts',(-39.8371685740842,30.2083333469893,-23.));
#10654=CARTESIAN_POINT('Ctrl Pts',(-33.6743371481684,30.0000000136559,-33.6743371481684));
#10655=CARTESIAN_POINT('Ctrl Pts',(-23.,29.7916666803226,-39.8371685740842));
#10656=CARTESIAN_POINT('Ctrl Pts',(-12.3256628518317,29.5833333469893,-46.));
#10657=CARTESIAN_POINT('Ctrl Pts',(-2.81668763803891E-15,29.3750000136559,
-46.));
#10658=CARTESIAN_POINT('Ctrl Pts',(12.3256628518316,29.1666666803226,-46.));
#10659=CARTESIAN_POINT('Ctrl Pts',(23.,28.9583333469893,-39.8371685740842));
#10660=CARTESIAN_POINT('Ctrl Pts',(33.6743371481683,28.7500000136559,-33.6743371481684));
#10661=CARTESIAN_POINT('Ctrl Pts',(39.8371685740842,28.5416666803226,-23.));
#10662=CARTESIAN_POINT('Ctrl Pts',(46.,28.3333333469893,-12.3256628518317));
#10663=CARTESIAN_POINT('Ctrl Pts',(46.,28.1250000136559,-5.63337527607782E-15));
#10664=CARTESIAN_POINT('Ctrl Pts',(46.,27.9166666803226,12.3256628518316));
#10665=CARTESIAN_POINT('Ctrl Pts',(39.8371685740842,27.7083333469893,23.));
#10666=CARTESIAN_POINT('Ctrl Pts',(33.6743371481684,27.5000000136559,33.6743371481683));
#10667=CARTESIAN_POINT('Ctrl Pts',(23.,27.2916666803226,39.8371685740842));
#10668=CARTESIAN_POINT('Ctrl Pts',(12.3256628518317,27.0833333469893,46.));
#10669=CARTESIAN_POINT('Ctrl Pts',(8.45006291411674E-15,26.8750000136559,
46.));
#10670=CARTESIAN_POINT('Ctrl Pts',(-12.3256628518316,26.6666666803226,46.));
#10671=CARTESIAN_POINT('Ctrl Pts',(-23.,26.4583333469893,39.8371685740842));
#10672=CARTESIAN_POINT('Ctrl Pts',(-33.6743371481683,26.2500000136559,33.6743371481684));
#10673=CARTESIAN_POINT('Ctrl Pts',(-39.8371685740842,26.0416666803226,23.));
#10674=CARTESIAN_POINT('Ctrl Pts',(-46.,25.8333333469893,12.3256628518317));
#10675=CARTESIAN_POINT('Ctrl Pts',(-46.,25.6250000136559,0.));
#10676=CARTESIAN_POINT('Ctrl Pts',(-48.706329375,57.187500006828,-1.8898197019151E-14));
#10677=CARTESIAN_POINT('Ctrl Pts',(-48.706329375,56.9791666734946,-13.0508216223155));
#10678=CARTESIAN_POINT('Ctrl Pts',(-42.1809185638422,56.7708333401613,-24.3531646875));
#10679=CARTESIAN_POINT('Ctrl Pts',(-35.6555077526845,56.562500006828,-35.6555077526845));
#10680=CARTESIAN_POINT('Ctrl Pts',(-24.3531646875,56.3541666734946,-42.1809185638423));
#10681=CARTESIAN_POINT('Ctrl Pts',(-13.0508216223155,56.1458333401613,-48.706329375));
#10682=CARTESIAN_POINT('Ctrl Pts',(1.59157945007855E-14,55.937500006828,
-48.706329375));
#10683=CARTESIAN_POINT('Ctrl Pts',(13.0508216223155,55.7291666734946,-48.706329375));
#10684=CARTESIAN_POINT('Ctrl Pts',(24.3531646875,55.5208333401613,-42.1809185638422));
#10685=CARTESIAN_POINT('Ctrl Pts',(35.6555077526845,55.312500006828,-35.6555077526845));
#10686=CARTESIAN_POINT('Ctrl Pts',(42.1809185638422,55.1041666734946,-24.3531646875));
#10687=CARTESIAN_POINT('Ctrl Pts',(48.706329375,54.8958333401613,-13.0508216223155));
#10688=CARTESIAN_POINT('Ctrl Pts',(48.706329375,54.687500006828,1.293339198242E-14));
#10689=CARTESIAN_POINT('Ctrl Pts',(48.706329375,54.4791666734946,13.0508216223155));
#10690=CARTESIAN_POINT('Ctrl Pts',(42.1809185638422,54.2708333401613,24.3531646875));
#10691=CARTESIAN_POINT('Ctrl Pts',(35.6555077526845,54.062500006828,35.6555077526845));
#10692=CARTESIAN_POINT('Ctrl Pts',(24.3531646875,53.8541666734946,42.1809185638422));
#10693=CARTESIAN_POINT('Ctrl Pts',(13.0508216223155,53.6458333401613,48.706329375));
#10694=CARTESIAN_POINT('Ctrl Pts',(-9.95098946405443E-15,53.437500006828,
48.706329375));
#10695=CARTESIAN_POINT('Ctrl Pts',(-13.0508216223155,53.2291666734946,48.706329375));
#10696=CARTESIAN_POINT('Ctrl Pts',(-24.3531646875,53.0208333401613,42.1809185638423));
#10697=CARTESIAN_POINT('Ctrl Pts',(-35.6555077526845,52.812500006828,35.6555077526845));
#10698=CARTESIAN_POINT('Ctrl Pts',(-42.1809185638422,52.6041666734946,24.3531646875));
#10699=CARTESIAN_POINT('Ctrl Pts',(-48.706329375,52.3958333401613,13.0508216223155));
#10700=CARTESIAN_POINT('Ctrl Pts',(-48.706329375,52.187500006828,-1.8898197019151E-14));
#10701=CARTESIAN_POINT('Ctrl Pts',(-48.706329375,51.9791666734946,-13.0508216223155));
#10702=CARTESIAN_POINT('Ctrl Pts',(-42.1809185638422,51.7708333401613,-24.3531646875));
#10703=CARTESIAN_POINT('Ctrl Pts',(-35.6555077526845,51.562500006828,-35.6555077526845));
#10704=CARTESIAN_POINT('Ctrl Pts',(-24.3531646875,51.3541666734946,-42.1809185638423));
#10705=CARTESIAN_POINT('Ctrl Pts',(-13.0508216223155,51.1458333401613,-48.706329375));
#10706=CARTESIAN_POINT('Ctrl Pts',(1.59157945007855E-14,50.937500006828,
-48.706329375));
#10707=CARTESIAN_POINT('Ctrl Pts',(13.0508216223155,50.7291666734946,-48.706329375));
#10708=CARTESIAN_POINT('Ctrl Pts',(24.3531646875,50.5208333401613,-42.1809185638422));
#10709=CARTESIAN_POINT('Ctrl Pts',(35.6555077526845,50.312500006828,-35.6555077526845));
#10710=CARTESIAN_POINT('Ctrl Pts',(42.1809185638422,50.1041666734946,-24.3531646875));
#10711=CARTESIAN_POINT('Ctrl Pts',(48.706329375,49.8958333401613,-13.0508216223155));
#10712=CARTESIAN_POINT('Ctrl Pts',(48.706329375,49.687500006828,1.293339198242E-14));
#10713=CARTESIAN_POINT('Ctrl Pts',(48.706329375,49.4791666734946,13.0508216223155));
#10714=CARTESIAN_POINT('Ctrl Pts',(42.1809185638422,49.2708333401613,24.3531646875));
#10715=CARTESIAN_POINT('Ctrl Pts',(35.6555077526845,49.062500006828,35.6555077526845));
#10716=CARTESIAN_POINT('Ctrl Pts',(24.3531646875,48.8541666734946,42.1809185638422));
#10717=CARTESIAN_POINT('Ctrl Pts',(13.0508216223155,48.6458333401613,48.706329375));
#10718=CARTESIAN_POINT('Ctrl Pts',(-9.95098946405443E-15,48.437500006828,
48.706329375));
#10719=CARTESIAN_POINT('Ctrl Pts',(-13.0508216223155,48.2291666734946,48.706329375));
#10720=CARTESIAN_POINT('Ctrl Pts',(-24.3531646875,48.0208333401613,42.1809185638423));
#10721=CARTESIAN_POINT('Ctrl Pts',(-35.6555077526845,47.812500006828,35.6555077526845));
#10722=CARTESIAN_POINT('Ctrl Pts',(-42.1809185638422,47.6041666734946,24.3531646875));
#10723=CARTESIAN_POINT('Ctrl Pts',(-48.706329375,47.3958333401613,13.0508216223155));
#10724=CARTESIAN_POINT('Ctrl Pts',(-48.706329375,47.187500006828,-1.8898197019151E-14));
#10725=CARTESIAN_POINT('Ctrl Pts',(-48.706329375,46.9791666734946,-13.0508216223155));
#10726=CARTESIAN_POINT('Ctrl Pts',(-42.1809185638422,46.7708333401613,-24.3531646875));
#10727=CARTESIAN_POINT('Ctrl Pts',(-35.6555077526845,46.562500006828,-35.6555077526845));
#10728=CARTESIAN_POINT('Ctrl Pts',(-24.3531646875,46.3541666734946,-42.1809185638423));
#10729=CARTESIAN_POINT('Ctrl Pts',(-13.0508216223155,46.1458333401613,-48.706329375));
#10730=CARTESIAN_POINT('Ctrl Pts',(1.59157945007855E-14,45.937500006828,
-48.706329375));
#10731=CARTESIAN_POINT('Ctrl Pts',(13.0508216223155,45.7291666734946,-48.706329375));
#10732=CARTESIAN_POINT('Ctrl Pts',(24.3531646875,45.5208333401613,-42.1809185638422));
#10733=CARTESIAN_POINT('Ctrl Pts',(35.6555077526845,45.312500006828,-35.6555077526845));
#10734=CARTESIAN_POINT('Ctrl Pts',(42.1809185638422,45.1041666734946,-24.3531646875));
#10735=CARTESIAN_POINT('Ctrl Pts',(48.706329375,44.8958333401613,-13.0508216223155));
#10736=CARTESIAN_POINT('Ctrl Pts',(48.706329375,44.687500006828,1.293339198242E-14));
#10737=CARTESIAN_POINT('Ctrl Pts',(48.706329375,44.4791666734946,13.0508216223155));
#10738=CARTESIAN_POINT('Ctrl Pts',(42.1809185638422,44.2708333401613,24.3531646875));
#10739=CARTESIAN_POINT('Ctrl Pts',(35.6555077526845,44.062500006828,35.6555077526845));
#10740=CARTESIAN_POINT('Ctrl Pts',(24.3531646875,43.8541666734946,42.1809185638422));
#10741=CARTESIAN_POINT('Ctrl Pts',(13.0508216223155,43.6458333401613,48.706329375));
#10742=CARTESIAN_POINT('Ctrl Pts',(-9.95098946405443E-15,43.437500006828,
48.706329375));
#10743=CARTESIAN_POINT('Ctrl Pts',(-13.0508216223155,43.2291666734946,48.706329375));
#10744=CARTESIAN_POINT('Ctrl Pts',(-24.3531646875,43.0208333401613,42.1809185638423));
#10745=CARTESIAN_POINT('Ctrl Pts',(-35.6555077526845,42.812500006828,35.6555077526845));
#10746=CARTESIAN_POINT('Ctrl Pts',(-42.1809185638422,42.6041666734946,24.3531646875));
#10747=CARTESIAN_POINT('Ctrl Pts',(-48.706329375,42.3958333401613,13.0508216223155));
#10748=CARTESIAN_POINT('Ctrl Pts',(-48.706329375,42.187500006828,-1.8898197019151E-14));
#10749=CARTESIAN_POINT('Ctrl Pts',(-48.706329375,41.9791666734946,-13.0508216223155));
#10750=CARTESIAN_POINT('Ctrl Pts',(-42.1809185638422,41.7708333401613,-24.3531646875));
#10751=CARTESIAN_POINT('Ctrl Pts',(-35.6555077526845,41.562500006828,-35.6555077526845));
#10752=CARTESIAN_POINT('Ctrl Pts',(-24.3531646875,41.3541666734946,-42.1809185638423));
#10753=CARTESIAN_POINT('Ctrl Pts',(-13.0508216223155,41.1458333401613,-48.706329375));
#10754=CARTESIAN_POINT('Ctrl Pts',(1.59157945007855E-14,40.937500006828,
-48.706329375));
#10755=CARTESIAN_POINT('Ctrl Pts',(13.0508216223155,40.7291666734946,-48.706329375));
#10756=CARTESIAN_POINT('Ctrl Pts',(24.3531646875,40.5208333401613,-42.1809185638422));
#10757=CARTESIAN_POINT('Ctrl Pts',(35.6555077526845,40.312500006828,-35.6555077526845));
#10758=CARTESIAN_POINT('Ctrl Pts',(42.1809185638422,40.1041666734946,-24.3531646875));
#10759=CARTESIAN_POINT('Ctrl Pts',(48.706329375,39.8958333401613,-13.0508216223155));
#10760=CARTESIAN_POINT('Ctrl Pts',(48.706329375,39.687500006828,1.293339198242E-14));
#10761=CARTESIAN_POINT('Ctrl Pts',(48.706329375,39.4791666734946,13.0508216223155));
#10762=CARTESIAN_POINT('Ctrl Pts',(42.1809185638422,39.2708333401613,24.3531646875));
#10763=CARTESIAN_POINT('Ctrl Pts',(35.6555077526845,39.062500006828,35.6555077526845));
#10764=CARTESIAN_POINT('Ctrl Pts',(24.3531646875,38.8541666734946,42.1809185638422));
#10765=CARTESIAN_POINT('Ctrl Pts',(13.0508216223155,38.6458333401613,48.706329375));
#10766=CARTESIAN_POINT('Ctrl Pts',(-9.95098946405443E-15,38.437500006828,
48.706329375));
#10767=CARTESIAN_POINT('Ctrl Pts',(-13.0508216223155,38.2291666734946,48.706329375));
#10768=CARTESIAN_POINT('Ctrl Pts',(-24.3531646875,38.0208333401613,42.1809185638423));
#10769=CARTESIAN_POINT('Ctrl Pts',(-35.6555077526845,37.812500006828,35.6555077526845));
#10770=CARTESIAN_POINT('Ctrl Pts',(-42.1809185638422,37.6041666734946,24.3531646875));
#10771=CARTESIAN_POINT('Ctrl Pts',(-48.706329375,37.3958333401613,13.0508216223155));
#10772=CARTESIAN_POINT('Ctrl Pts',(-48.706329375,37.187500006828,-1.8898197019151E-14));
#10773=CARTESIAN_POINT('Ctrl Pts',(-48.706329375,36.9791666734946,-13.0508216223155));
#10774=CARTESIAN_POINT('Ctrl Pts',(-42.1809185638422,36.7708333401613,-24.3531646875));
#10775=CARTESIAN_POINT('Ctrl Pts',(-35.6555077526845,36.562500006828,-35.6555077526845));
#10776=CARTESIAN_POINT('Ctrl Pts',(-24.3531646875,36.3541666734946,-42.1809185638423));
#10777=CARTESIAN_POINT('Ctrl Pts',(-13.0508216223155,36.1458333401613,-48.706329375));
#10778=CARTESIAN_POINT('Ctrl Pts',(1.59157945007855E-14,35.937500006828,
-48.706329375));
#10779=CARTESIAN_POINT('Ctrl Pts',(13.0508216223155,35.7291666734946,-48.706329375));
#10780=CARTESIAN_POINT('Ctrl Pts',(24.3531646875,35.5208333401613,-42.1809185638422));
#10781=CARTESIAN_POINT('Ctrl Pts',(35.6555077526845,35.312500006828,-35.6555077526845));
#10782=CARTESIAN_POINT('Ctrl Pts',(42.1809185638422,35.1041666734946,-24.3531646875));
#10783=CARTESIAN_POINT('Ctrl Pts',(48.706329375,34.8958333401613,-13.0508216223155));
#10784=CARTESIAN_POINT('Ctrl Pts',(48.706329375,34.687500006828,1.293339198242E-14));
#10785=CARTESIAN_POINT('Ctrl Pts',(48.706329375,34.4791666734946,13.0508216223155));
#10786=CARTESIAN_POINT('Ctrl Pts',(42.1809185638422,34.2708333401613,24.3531646875));
#10787=CARTESIAN_POINT('Ctrl Pts',(35.6555077526845,34.062500006828,35.6555077526845));
#10788=CARTESIAN_POINT('Ctrl Pts',(24.3531646875,33.8541666734946,42.1809185638422));
#10789=CARTESIAN_POINT('Ctrl Pts',(13.0508216223155,33.6458333401613,48.706329375));
#10790=CARTESIAN_POINT('Ctrl Pts',(-9.95098946405443E-15,33.437500006828,
48.706329375));
#10791=CARTESIAN_POINT('Ctrl Pts',(-13.0508216223155,33.2291666734946,48.706329375));
#10792=CARTESIAN_POINT('Ctrl Pts',(-24.3531646875,33.0208333401613,42.1809185638423));
#10793=CARTESIAN_POINT('Ctrl Pts',(-35.6555077526845,32.812500006828,35.6555077526845));
#10794=CARTESIAN_POINT('Ctrl Pts',(-42.1809185638422,32.6041666734946,24.3531646875));
#10795=CARTESIAN_POINT('Ctrl Pts',(-48.706329375,32.3958333401613,13.0508216223155));
#10796=CARTESIAN_POINT('Ctrl Pts',(-48.706329375,32.187500006828,-1.8898197019151E-14));
#10797=CARTESIAN_POINT('Ctrl Pts',(-48.706329375,31.9791666734946,-13.0508216223155));
#10798=CARTESIAN_POINT('Ctrl Pts',(-42.1809185638422,31.7708333401613,-24.3531646875));
#10799=CARTESIAN_POINT('Ctrl Pts',(-35.6555077526845,31.562500006828,-35.6555077526845));
#10800=CARTESIAN_POINT('Ctrl Pts',(-24.3531646875,31.3541666734946,-42.1809185638423));
#10801=CARTESIAN_POINT('Ctrl Pts',(-13.0508216223155,31.1458333401613,-48.706329375));
#10802=CARTESIAN_POINT('Ctrl Pts',(1.59157945007855E-14,30.937500006828,
-48.706329375));
#10803=CARTESIAN_POINT('Ctrl Pts',(13.0508216223155,30.7291666734946,-48.706329375));
#10804=CARTESIAN_POINT('Ctrl Pts',(24.3531646875,30.5208333401613,-42.1809185638422));
#10805=CARTESIAN_POINT('Ctrl Pts',(35.6555077526845,30.312500006828,-35.6555077526845));
#10806=CARTESIAN_POINT('Ctrl Pts',(42.1809185638422,30.1041666734946,-24.3531646875));
#10807=CARTESIAN_POINT('Ctrl Pts',(48.706329375,29.8958333401613,-13.0508216223155));
#10808=CARTESIAN_POINT('Ctrl Pts',(48.706329375,29.687500006828,1.293339198242E-14));
#10809=CARTESIAN_POINT('Ctrl Pts',(48.706329375,29.4791666734946,13.0508216223155));
#10810=CARTESIAN_POINT('Ctrl Pts',(42.1809185638422,29.2708333401613,24.3531646875));
#10811=CARTESIAN_POINT('Ctrl Pts',(35.6555077526845,29.062500006828,35.6555077526845));
#10812=CARTESIAN_POINT('Ctrl Pts',(24.3531646875,28.8541666734946,42.1809185638422));
#10813=CARTESIAN_POINT('Ctrl Pts',(13.0508216223155,28.6458333401613,48.706329375));
#10814=CARTESIAN_POINT('Ctrl Pts',(-9.95098946405443E-15,28.437500006828,
48.706329375));
#10815=CARTESIAN_POINT('Ctrl Pts',(-13.0508216223155,28.2291666734946,48.706329375));
#10816=CARTESIAN_POINT('Ctrl Pts',(-24.3531646875,28.0208333401613,42.1809185638423));
#10817=CARTESIAN_POINT('Ctrl Pts',(-35.6555077526845,27.812500006828,35.6555077526845));
#10818=CARTESIAN_POINT('Ctrl Pts',(-42.1809185638422,27.6041666734946,24.3531646875));
#10819=CARTESIAN_POINT('Ctrl Pts',(-48.706329375,27.3958333401613,13.0508216223155));
#10820=CARTESIAN_POINT('Ctrl Pts',(-48.706329375,27.187500006828,-1.8898197019151E-14));
#10821=CARTESIAN_POINT('',(-4.32456003949875,38.3676432269777,48.5139639861634));
#10822=CARTESIAN_POINT('',(-48.5725845633798,37.2456516907297,3.60701400320327));
#10823=CARTESIAN_POINT('Ctrl Pts',(-4.32456003949875,38.3676432269777,48.5139639861634));
#10824=CARTESIAN_POINT('Ctrl Pts',(-15.038141415499,38.1925348924095,47.5589497574396));
#10825=CARTESIAN_POINT('Ctrl Pts',(-24.3531646875,38.0208333401613,42.1809185638423));
#10826=CARTESIAN_POINT('Ctrl Pts',(-35.6555077526845,37.812500006828,35.6555077526845));
#10827=CARTESIAN_POINT('Ctrl Pts',(-42.1809185638422,37.6041666734946,24.3531646875));
#10828=CARTESIAN_POINT('Ctrl Pts',(-47.7480251419552,37.4264286116308,14.7106532430575));
#10829=CARTESIAN_POINT('Ctrl Pts',(-48.5725845633798,37.2456516907297,3.60701400320327));
#10830=CARTESIAN_POINT('',(-45.858362923034,35.686608693912,3.60701400320327));
#10831=CARTESIAN_POINT('Ctrl Pts',(-48.5725845633798,37.2456516907297,3.60701400320327));
#10832=CARTESIAN_POINT('Ctrl Pts',(-48.3407853679392,37.1124685639422,3.60701400320327));
#10833=CARTESIAN_POINT('Ctrl Pts',(-48.1089821836664,36.9792923792741,3.60701400320327));
#10834=CARTESIAN_POINT('Ctrl Pts',(-47.6453674864979,36.7129545080418,3.60701400320327));
#10835=CARTESIAN_POINT('Ctrl Pts',(-47.4135559734254,36.5797928212585,3.60701400320327));
#10836=CARTESIAN_POINT('Ctrl Pts',(-47.1817401099609,36.4466387085919,3.60701400320327));
#10837=CARTESIAN_POINT('Ctrl Pts',(-46.7406305897488,36.1932671494809,3.60701400320327));
#10838=CARTESIAN_POINT('Ctrl Pts',(-46.2995053259033,35.9399229970588,3.60701400320328));
#10839=CARTESIAN_POINT('Ctrl Pts',(-45.858362923034,35.686608693912,3.60701400320327));
#10840=CARTESIAN_POINT('',(-4.32199731091469,36.8010262662206,45.796510120799));
#10841=CARTESIAN_POINT('Ctrl Pts',(-4.32199731091469,36.8010262662206,45.796510120799));
#10842=CARTESIAN_POINT('Ctrl Pts',(-14.3109099936784,36.6279201849842,44.8538170282468));
#10843=CARTESIAN_POINT('Ctrl Pts',(-23.,36.4583333469893,39.8371685740842));
#10844=CARTESIAN_POINT('Ctrl Pts',(-33.6743371481683,36.2500000136559,33.6743371481684));
#10845=CARTESIAN_POINT('Ctrl Pts',(-39.8371685740842,36.0416666803226,23.));
#10846=CARTESIAN_POINT('Ctrl Pts',(-45.0420919829705,35.8657152436245,13.9848082063043));
#10847=CARTESIAN_POINT('Ctrl Pts',(-45.858362923034,35.686608693912,3.60701400320327));
#10848=CARTESIAN_POINT('',(-4.32456320853981,36.9438035983166,46.0440414573356));
#10849=CARTESIAN_POINT('Origin',(11.5422763248982,36.5066019508688,46.295943288233));
#10850=CARTESIAN_POINT('Ctrl Pts',(-4.32456003949885,36.9438034227513,46.0440415585359));
#10851=CARTESIAN_POINT('Ctrl Pts',(-4.32456003949885,37.1552503030329,46.4108661087096));
#10852=CARTESIAN_POINT('Ctrl Pts',(-4.32456003949594,37.3667894036306,46.7778368059273));
#10853=CARTESIAN_POINT('Ctrl Pts',(-4.32456003949594,37.8413187510542,47.6010049167753));
#10854=CARTESIAN_POINT('Ctrl Pts',(-4.32456003949875,38.1045569543834,48.057625392756));
#10855=CARTESIAN_POINT('Ctrl Pts',(-4.32456003949875,38.3676432269777,48.5139639861634));
#10856=CARTESIAN_POINT('Origin',(-7.99360577730113E-14,57.8125000068276,
4.34631818602828E-14));
#10857=CARTESIAN_POINT('',(3.61292728433799,57.1292520480092,-48.5721450795008));
#10858=CARTESIAN_POINT('',(48.5134353784344,56.0074536451604,-4.33048599679673));
#10859=CARTESIAN_POINT('Ctrl Pts',(3.61292728433799,57.1292520480093,-48.5721450795008));
#10860=CARTESIAN_POINT('Ctrl Pts',(14.7133549689477,56.9485216017707,-47.7464652997852));
#10861=CARTESIAN_POINT('Ctrl Pts',(24.3531646875,56.7708333401613,-42.1809185638422));
#10862=CARTESIAN_POINT('Ctrl Pts',(35.6555077526845,56.562500006828,-35.6555077526845));
#10863=CARTESIAN_POINT('Ctrl Pts',(42.1809185638422,56.3541666734946,-24.3531646875));
#10864=CARTESIAN_POINT('Ctrl Pts',(47.5573898704235,56.1825149229327,-15.0408432190651));
#10865=CARTESIAN_POINT('Ctrl Pts',(48.5134353784344,56.0074536451604,-4.33048599679673));
#10866=CARTESIAN_POINT('',(48.5134353784344,56.0074536451604,-4.33048599679673));
#10867=CARTESIAN_POINT('',(3.61292728433799,55.8792520480092,-48.5721450795008));
#10868=CARTESIAN_POINT('Origin',(-7.99360577730113E-14,57.8125000068276,
4.34631818602828E-14));
#10869=CARTESIAN_POINT('',(48.5725845633798,55.8793483229262,3.60701400320328));
#10870=CARTESIAN_POINT('',(48.5725845633798,54.6293483229262,3.60701400320328));
#10871=CARTESIAN_POINT('',(3.612927284338,54.7457479656467,48.5721450795008));
#10872=CARTESIAN_POINT('Ctrl Pts',(48.5725845633798,55.8793483229262,3.60701400320328));
#10873=CARTESIAN_POINT('Ctrl Pts',(47.7480251419552,55.6985714020251,14.7106532430575));
#10874=CARTESIAN_POINT('Ctrl Pts',(42.1809185638422,55.5208333401613,24.3531646875));
#10875=CARTESIAN_POINT('Ctrl Pts',(35.6555077526845,55.312500006828,35.6555077526845));
#10876=CARTESIAN_POINT('Ctrl Pts',(24.3531646875,55.1041666734946,42.1809185638422));
#10877=CARTESIAN_POINT('Ctrl Pts',(14.7133549689477,54.9264784118853,47.7464652997852));
#10878=CARTESIAN_POINT('Ctrl Pts',(3.612927284338,54.7457479656467,48.5721450795008));
#10879=CARTESIAN_POINT('',(3.612927284338,54.7457479656467,48.5721450795008));
#10880=CARTESIAN_POINT('Origin',(-7.99360577730113E-14,57.8125000068276,
4.34631818602828E-14));
#10881=CARTESIAN_POINT('',(3.612927284338,52.1292520480092,-48.5721450795008));
#10882=CARTESIAN_POINT('',(48.5134353784344,51.0074536451604,-4.33048599679671));
#10883=CARTESIAN_POINT('Ctrl Pts',(3.612927284338,52.1292520480092,-48.5721450795008));
#10884=CARTESIAN_POINT('Ctrl Pts',(14.7133549689477,51.9485216017707,-47.7464652997852));
#10885=CARTESIAN_POINT('Ctrl Pts',(24.3531646875,51.7708333401613,-42.1809185638422));
#10886=CARTESIAN_POINT('Ctrl Pts',(35.6555077526845,51.562500006828,-35.6555077526845));
#10887=CARTESIAN_POINT('Ctrl Pts',(42.1809185638422,51.3541666734946,-24.3531646875));
#10888=CARTESIAN_POINT('Ctrl Pts',(47.5573898704235,51.1825149229327,-15.0408432190651));
#10889=CARTESIAN_POINT('Ctrl Pts',(48.5134353784344,51.0074536451604,-4.33048599679671));
#10890=CARTESIAN_POINT('',(48.5134353784344,51.0074536451604,-4.33048599679671));
#10891=CARTESIAN_POINT('',(3.612927284338,50.8792520480092,-48.5721450795008));
#10892=CARTESIAN_POINT('Origin',(-7.99360577730113E-14,57.8125000068276,
4.34631818602828E-14));
#10893=CARTESIAN_POINT('',(48.5725845633798,50.8793483229262,3.60701400320328));
#10894=CARTESIAN_POINT('',(48.5725845633798,49.6293483229262,3.60701400320328));
#10895=CARTESIAN_POINT('',(3.61292728433797,49.7457479656467,48.5721450795008));
#10896=CARTESIAN_POINT('Ctrl Pts',(48.5725845633798,50.8793483229262,3.60701400320328));
#10897=CARTESIAN_POINT('Ctrl Pts',(47.7480251419552,50.6985714020251,14.7106532430575));
#10898=CARTESIAN_POINT('Ctrl Pts',(42.1809185638422,50.5208333401613,24.3531646875));
#10899=CARTESIAN_POINT('Ctrl Pts',(35.6555077526845,50.312500006828,35.6555077526845));
#10900=CARTESIAN_POINT('Ctrl Pts',(24.3531646875,50.1041666734946,42.1809185638422));
#10901=CARTESIAN_POINT('Ctrl Pts',(14.7133549689477,49.9264784118853,47.7464652997852));
#10902=CARTESIAN_POINT('Ctrl Pts',(3.61292728433797,49.7457479656467,48.5721450795008));
#10903=CARTESIAN_POINT('',(3.61292728433797,49.7457479656467,48.5721450795008));
#10904=CARTESIAN_POINT('Origin',(-7.99360577730113E-14,57.8125000068276,
4.34631818602828E-14));
#10905=CARTESIAN_POINT('',(3.61292728433799,47.1292520480092,-48.5721450795008));
#10906=CARTESIAN_POINT('',(48.5134353784344,46.0074536451604,-4.33048599679671));
#10907=CARTESIAN_POINT('Ctrl Pts',(3.61292728433799,47.1292520480092,-48.5721450795008));
#10908=CARTESIAN_POINT('Ctrl Pts',(14.7133549689477,46.9485216017706,-47.7464652997852));
#10909=CARTESIAN_POINT('Ctrl Pts',(24.3531646875,46.7708333401613,-42.1809185638422));
#10910=CARTESIAN_POINT('Ctrl Pts',(35.6555077526845,46.562500006828,-35.6555077526845));
#10911=CARTESIAN_POINT('Ctrl Pts',(42.1809185638422,46.3541666734946,-24.3531646875));
#10912=CARTESIAN_POINT('Ctrl Pts',(47.5573898704235,46.1825149229327,-15.0408432190651));
#10913=CARTESIAN_POINT('Ctrl Pts',(48.5134353784344,46.0074536451604,-4.33048599679671));
#10914=CARTESIAN_POINT('',(48.5134353784344,46.0074536451604,-4.33048599679671));
#10915=CARTESIAN_POINT('',(3.61292728433799,45.8792520480092,-48.5721450795008));
#10916=CARTESIAN_POINT('Origin',(-7.99360577730113E-14,57.8125000068276,
4.34631818602828E-14));
#10917=CARTESIAN_POINT('',(48.5725845633798,45.8793483229262,3.60701400320328));
#10918=CARTESIAN_POINT('',(48.5725845633798,44.6293483229262,3.60701400320328));
#10919=CARTESIAN_POINT('',(3.61292728433797,44.7457479656467,48.5721450795008));
#10920=CARTESIAN_POINT('Ctrl Pts',(48.5725845633798,45.8793483229262,3.60701400320328));
#10921=CARTESIAN_POINT('Ctrl Pts',(47.7480251419552,45.6985714020251,14.7106532430575));
#10922=CARTESIAN_POINT('Ctrl Pts',(42.1809185638422,45.5208333401613,24.3531646875));
#10923=CARTESIAN_POINT('Ctrl Pts',(35.6555077526845,45.312500006828,35.6555077526845));
#10924=CARTESIAN_POINT('Ctrl Pts',(24.3531646875,45.1041666734946,42.1809185638422));
#10925=CARTESIAN_POINT('Ctrl Pts',(14.7133549689477,44.9264784118853,47.7464652997852));
#10926=CARTESIAN_POINT('Ctrl Pts',(3.61292728433797,44.7457479656467,48.5721450795008));
#10927=CARTESIAN_POINT('',(3.61292728433797,44.7457479656467,48.5721450795008));
#10928=CARTESIAN_POINT('Origin',(-7.99360577730113E-14,57.8125000068276,
4.34631818602828E-14));
#10929=CARTESIAN_POINT('',(3.61292728433798,42.1292520480093,-48.5721450795008));
#10930=CARTESIAN_POINT('',(48.5134353784344,41.0074536451604,-4.33048599679679));
#10931=CARTESIAN_POINT('Ctrl Pts',(3.61292728433798,42.1292520480093,-48.5721450795008));
#10932=CARTESIAN_POINT('Ctrl Pts',(14.7133549689477,41.9485216017706,-47.7464652997852));
#10933=CARTESIAN_POINT('Ctrl Pts',(24.3531646875,41.7708333401613,-42.1809185638422));
#10934=CARTESIAN_POINT('Ctrl Pts',(35.6555077526845,41.562500006828,-35.6555077526845));
#10935=CARTESIAN_POINT('Ctrl Pts',(42.1809185638422,41.3541666734946,-24.3531646875));
#10936=CARTESIAN_POINT('Ctrl Pts',(47.5573898704235,41.1825149229327,-15.0408432190651));
#10937=CARTESIAN_POINT('Ctrl Pts',(48.5134353784344,41.0074536451604,-4.33048599679679));
#10938=CARTESIAN_POINT('',(48.5134353784344,41.0074536451604,-4.33048599679679));
#10939=CARTESIAN_POINT('',(3.61292728433798,40.8792520480093,-48.5721450795008));
#10940=CARTESIAN_POINT('Origin',(-7.99360577730113E-14,57.8125000068276,
4.34631818602828E-14));
#10941=CARTESIAN_POINT('',(48.5725845633798,40.8793483229262,3.60701400320329));
#10942=CARTESIAN_POINT('',(48.5725845633798,39.6293483229262,3.60701400320329));
#10943=CARTESIAN_POINT('',(3.61292728433799,39.7457479656467,48.5721450795008));
#10944=CARTESIAN_POINT('Ctrl Pts',(48.5725845633798,40.8793483229262,3.60701400320329));
#10945=CARTESIAN_POINT('Ctrl Pts',(47.7480251419552,40.6985714020251,14.7106532430575));
#10946=CARTESIAN_POINT('Ctrl Pts',(42.1809185638422,40.5208333401613,24.3531646875));
#10947=CARTESIAN_POINT('Ctrl Pts',(35.6555077526845,40.312500006828,35.6555077526845));
#10948=CARTESIAN_POINT('Ctrl Pts',(24.3531646875,40.1041666734946,42.1809185638422));
#10949=CARTESIAN_POINT('Ctrl Pts',(14.7133549689477,39.9264784118853,47.7464652997852));
#10950=CARTESIAN_POINT('Ctrl Pts',(3.61292728433799,39.7457479656467,48.5721450795008));
#10951=CARTESIAN_POINT('',(3.61292728433799,39.7457479656467,48.5721450795008));
#10952=CARTESIAN_POINT('Origin',(-7.99360577730113E-14,57.8125000068276,
4.34631818602828E-14));
#10953=CARTESIAN_POINT('',(-48.5134353784345,58.3675463684955,-4.33048599679673));
#10954=CARTESIAN_POINT('',(-48.5134353784345,57.1175463684955,-4.33048599679673));
#10955=CARTESIAN_POINT('',(-4.32456003949879,57.2573567866782,-48.5139639861634));
#10956=CARTESIAN_POINT('Ctrl Pts',(-48.5134353784344,58.3675463684955,-4.33048599679673));
#10957=CARTESIAN_POINT('Ctrl Pts',(-47.5573898704235,58.1924850907233,-15.0408432190651));
#10958=CARTESIAN_POINT('Ctrl Pts',(-42.1809185638422,58.0208333401613,-24.3531646875));
#10959=CARTESIAN_POINT('Ctrl Pts',(-35.6555077526845,57.812500006828,-35.6555077526845));
#10960=CARTESIAN_POINT('Ctrl Pts',(-24.3531646875,57.6041666734946,-42.1809185638422));
#10961=CARTESIAN_POINT('Ctrl Pts',(-15.038141415499,57.4324651212465,-47.5589497574396));
#10962=CARTESIAN_POINT('Ctrl Pts',(-4.32456003949879,57.2573567866782,-48.5139639861634));
#10963=CARTESIAN_POINT('',(-4.32456003949879,57.2573567866783,-48.5139639861634));
#10964=CARTESIAN_POINT('Origin',(-7.99360577730113E-14,57.8125000068276,
4.34631818602828E-14));
#10965=CARTESIAN_POINT('',(-48.5134353784344,53.3675463684955,-4.33048599679673));
#10966=CARTESIAN_POINT('',(-48.5134353784345,52.1175463684955,-4.33048599679673));
#10967=CARTESIAN_POINT('',(-4.32456003949876,52.2573567866782,-48.5139639861634));
#10968=CARTESIAN_POINT('Ctrl Pts',(-48.5134353784344,53.3675463684955,-4.33048599679673));
#10969=CARTESIAN_POINT('Ctrl Pts',(-47.5573898704235,53.1924850907232,-15.0408432190651));
#10970=CARTESIAN_POINT('Ctrl Pts',(-42.1809185638422,53.0208333401613,-24.3531646875));
#10971=CARTESIAN_POINT('Ctrl Pts',(-35.6555077526845,52.812500006828,-35.6555077526845));
#10972=CARTESIAN_POINT('Ctrl Pts',(-24.3531646875,52.6041666734946,-42.1809185638422));
#10973=CARTESIAN_POINT('Ctrl Pts',(-15.038141415499,52.4324651212465,-47.5589497574396));
#10974=CARTESIAN_POINT('Ctrl Pts',(-4.32456003949876,52.2573567866783,-48.5139639861634));
#10975=CARTESIAN_POINT('',(-4.32456003949876,52.2573567866782,-48.5139639861634));
#10976=CARTESIAN_POINT('Origin',(-7.99360577730113E-14,57.8125000068276,
4.34631818602828E-14));
#10977=CARTESIAN_POINT('',(-4.32456003949878,54.6176432269777,48.5139639861634));
#10978=CARTESIAN_POINT('',(-48.5725845633798,53.4956516907298,3.60701400320327));
#10979=CARTESIAN_POINT('Ctrl Pts',(-4.32456003949878,54.6176432269777,48.5139639861634));
#10980=CARTESIAN_POINT('Ctrl Pts',(-15.038141415499,54.4425348924095,47.5589497574396));
#10981=CARTESIAN_POINT('Ctrl Pts',(-24.3531646875,54.2708333401613,42.1809185638423));
#10982=CARTESIAN_POINT('Ctrl Pts',(-35.6555077526845,54.062500006828,35.6555077526845));
#10983=CARTESIAN_POINT('Ctrl Pts',(-42.1809185638422,53.8541666734946,24.3531646875));
#10984=CARTESIAN_POINT('Ctrl Pts',(-47.7480251419551,53.6764286116308,14.7106532430575));
#10985=CARTESIAN_POINT('Ctrl Pts',(-48.5725845633798,53.4956516907298,3.60701400320327));
#10986=CARTESIAN_POINT('',(-48.5725845633798,53.4956516907298,3.60701400320327));
#10987=CARTESIAN_POINT('',(-4.32456003949878,53.3676432269777,48.5139639861634));
#10988=CARTESIAN_POINT('Origin',(-7.99360577730113E-14,57.8125000068276,
4.34631818602828E-14));
#10989=CARTESIAN_POINT('',(-48.5134353784344,48.3675463684955,-4.33048599679673));
#10990=CARTESIAN_POINT('',(-48.5134353784345,47.1175463684955,-4.33048599679673));
#10991=CARTESIAN_POINT('',(-4.32456003949881,47.2573567866782,-48.5139639861634));
#10992=CARTESIAN_POINT('Ctrl Pts',(-48.5134353784344,48.3675463684955,-4.33048599679673));
#10993=CARTESIAN_POINT('Ctrl Pts',(-47.5573898704235,48.1924850907233,-15.0408432190651));
#10994=CARTESIAN_POINT('Ctrl Pts',(-42.1809185638422,48.0208333401613,-24.3531646875));
#10995=CARTESIAN_POINT('Ctrl Pts',(-35.6555077526845,47.812500006828,-35.6555077526845));
#10996=CARTESIAN_POINT('Ctrl Pts',(-24.3531646875,47.6041666734946,-42.1809185638422));
#10997=CARTESIAN_POINT('Ctrl Pts',(-15.0381414154991,47.4324651212465,-47.5589497574396));
#10998=CARTESIAN_POINT('Ctrl Pts',(-4.32456003949881,47.2573567866782,-48.5139639861634));
#10999=CARTESIAN_POINT('',(-4.32456003949881,47.2573567866783,-48.5139639861634));
#11000=CARTESIAN_POINT('Origin',(-7.99360577730113E-14,57.8125000068276,
4.34631818602828E-14));
#11001=CARTESIAN_POINT('',(-4.32456003949883,49.6176432269777,48.5139639861634));
#11002=CARTESIAN_POINT('',(-48.5725845633798,48.4956516907297,3.60701400320326));
#11003=CARTESIAN_POINT('Ctrl Pts',(-4.32456003949883,49.6176432269777,48.5139639861634));
#11004=CARTESIAN_POINT('Ctrl Pts',(-15.0381414154991,49.4425348924095,47.5589497574396));
#11005=CARTESIAN_POINT('Ctrl Pts',(-24.3531646875,49.2708333401613,42.1809185638423));
#11006=CARTESIAN_POINT('Ctrl Pts',(-35.6555077526845,49.062500006828,35.6555077526845));
#11007=CARTESIAN_POINT('Ctrl Pts',(-42.1809185638422,48.8541666734946,24.3531646875));
#11008=CARTESIAN_POINT('Ctrl Pts',(-47.7480251419552,48.6764286116309,14.7106532430575));
#11009=CARTESIAN_POINT('Ctrl Pts',(-48.5725845633798,48.4956516907297,3.60701400320326));
#11010=CARTESIAN_POINT('',(-48.5725845633798,48.4956516907297,3.60701400320326));
#11011=CARTESIAN_POINT('',(-4.32456003949883,48.3676432269777,48.5139639861634));
#11012=CARTESIAN_POINT('Origin',(-7.99360577730113E-14,57.8125000068276,
4.34631818602828E-14));
#11013=CARTESIAN_POINT('',(-48.5134353784345,43.3675463684955,-4.33048599679665));
#11014=CARTESIAN_POINT('',(-48.5134353784345,42.1175463684956,-4.33048599679665));
#11015=CARTESIAN_POINT('',(-4.32456003949873,42.2573567866782,-48.5139639861634));
#11016=CARTESIAN_POINT('Ctrl Pts',(-48.5134353784345,43.3675463684955,-4.33048599679665));
#11017=CARTESIAN_POINT('Ctrl Pts',(-47.5573898704235,43.1924850907233,-15.040843219065));
#11018=CARTESIAN_POINT('Ctrl Pts',(-42.1809185638422,43.0208333401613,-24.3531646875));
#11019=CARTESIAN_POINT('Ctrl Pts',(-35.6555077526845,42.812500006828,-35.6555077526845));
#11020=CARTESIAN_POINT('Ctrl Pts',(-24.3531646875,42.6041666734946,-42.1809185638422));
#11021=CARTESIAN_POINT('Ctrl Pts',(-15.038141415499,42.4324651212465,-47.5589497574396));
#11022=CARTESIAN_POINT('Ctrl Pts',(-4.32456003949873,42.2573567866782,-48.5139639861634));
#11023=CARTESIAN_POINT('',(-4.32456003949873,42.2573567866783,-48.5139639861634));
#11024=CARTESIAN_POINT('Origin',(-7.99360577730113E-14,57.8125000068276,
4.34631818602828E-14));
#11025=CARTESIAN_POINT('',(-4.32456003949883,44.6176432269777,48.5139639861634));
#11026=CARTESIAN_POINT('',(-48.5725845633798,43.4956516907297,3.60701400320326));
#11027=CARTESIAN_POINT('Ctrl Pts',(-4.32456003949883,44.6176432269777,48.5139639861634));
#11028=CARTESIAN_POINT('Ctrl Pts',(-15.0381414154991,44.4425348924095,47.5589497574396));
#11029=CARTESIAN_POINT('Ctrl Pts',(-24.3531646875,44.2708333401613,42.1809185638423));
#11030=CARTESIAN_POINT('Ctrl Pts',(-35.6555077526845,44.062500006828,35.6555077526845));
#11031=CARTESIAN_POINT('Ctrl Pts',(-42.1809185638422,43.8541666734946,24.3531646875));
#11032=CARTESIAN_POINT('Ctrl Pts',(-47.7480251419552,43.6764286116309,14.7106532430575));
#11033=CARTESIAN_POINT('Ctrl Pts',(-48.5725845633798,43.4956516907297,3.60701400320326));
#11034=CARTESIAN_POINT('',(-48.5725845633798,43.4956516907297,3.60701400320326));
#11035=CARTESIAN_POINT('',(-4.32456003949883,43.3676432269777,48.5139639861634));
#11036=CARTESIAN_POINT('Origin',(-7.99360577730113E-14,57.8125000068276,
4.34631818602828E-14));
#11037=CARTESIAN_POINT('',(-48.5134353784344,38.3675463684955,-4.33048599679682));
#11038=CARTESIAN_POINT('',(-48.5134353784344,37.1175463684955,-4.33048599679682));
#11039=CARTESIAN_POINT('',(-4.32456003949869,37.2573567866782,-48.5139639861634));
#11040=CARTESIAN_POINT('Ctrl Pts',(-48.5134353784344,38.3675463684955,-4.33048599679682));
#11041=CARTESIAN_POINT('Ctrl Pts',(-47.5573898704235,38.1924850907232,-15.0408432190651));
#11042=CARTESIAN_POINT('Ctrl Pts',(-42.1809185638422,38.0208333401613,-24.3531646875));
#11043=CARTESIAN_POINT('Ctrl Pts',(-35.6555077526845,37.812500006828,-35.6555077526845));
#11044=CARTESIAN_POINT('Ctrl Pts',(-24.3531646875,37.6041666734946,-42.1809185638422));
#11045=CARTESIAN_POINT('Ctrl Pts',(-15.038141415499,37.4324651212465,-47.5589497574396));
#11046=CARTESIAN_POINT('Ctrl Pts',(-4.32456003949869,37.2573567866782,-48.5139639861634));
#11047=CARTESIAN_POINT('',(-4.32456320853981,36.9438035983105,-48.513963421183));
#11048=CARTESIAN_POINT('',(-4.32456003949878,37.2573567866782,-48.5139639861634));
#11049=CARTESIAN_POINT('Ctrl Pts',(-4.32456637758084,36.9438035983105,-48.5139634211829));
#11050=CARTESIAN_POINT('Ctrl Pts',(-4.32456637758084,36.6377267119794,-48.5139634211829));
#11051=CARTESIAN_POINT('Ctrl Pts',(-4.2883015397967,36.3188714657862,-48.5172427906022));
#11052=CARTESIAN_POINT('Ctrl Pts',(-4.21205777787802,36.0055185535965,-48.5238610423963));
#11053=CARTESIAN_POINT('Origin',(-7.99360577730113E-14,57.8125000068276,
4.34631818602828E-14));
#11054=CARTESIAN_POINT('',(-4.32456003949875,39.6176432269777,48.5139639861634));
#11055=CARTESIAN_POINT('',(-48.5725845633798,38.4956516907297,3.60701400320327));
#11056=CARTESIAN_POINT('Ctrl Pts',(-4.32456003949875,39.6176432269777,48.5139639861634));
#11057=CARTESIAN_POINT('Ctrl Pts',(-15.038141415499,39.4425348924095,47.5589497574396));
#11058=CARTESIAN_POINT('Ctrl Pts',(-24.3531646875,39.2708333401613,42.1809185638423));
#11059=CARTESIAN_POINT('Ctrl Pts',(-35.6555077526845,39.062500006828,35.6555077526845));
#11060=CARTESIAN_POINT('Ctrl Pts',(-42.1809185638422,38.8541666734946,24.3531646875));
#11061=CARTESIAN_POINT('Ctrl Pts',(-47.7480251419552,38.6764286116308,14.7106532430575));
#11062=CARTESIAN_POINT('Ctrl Pts',(-48.5725845633798,38.4956516907297,3.60701400320327));
#11063=CARTESIAN_POINT('',(-48.5725845633798,38.4956516907298,3.60701400320327));
#11064=CARTESIAN_POINT('',(-4.32456003949875,38.3676432269777,48.5139639861634));
#11065=CARTESIAN_POINT('Origin',(-7.99360577730113E-14,57.8125000068276,
4.34631818602828E-14));
#11066=CARTESIAN_POINT('',(3.61292728433801,37.1292520480092,-48.5721450795008));
#11067=CARTESIAN_POINT('',(48.5134353784344,36.0074536451604,-4.33048599679682));
#11068=CARTESIAN_POINT('Ctrl Pts',(3.61292728433801,37.1292520480092,-48.5721450795008));
#11069=CARTESIAN_POINT('Ctrl Pts',(14.7133549689477,36.9485216017706,-47.7464652997852));
#11070=CARTESIAN_POINT('Ctrl Pts',(24.3531646875,36.7708333401613,-42.1809185638422));
#11071=CARTESIAN_POINT('Ctrl Pts',(35.6555077526845,36.562500006828,-35.6555077526845));
#11072=CARTESIAN_POINT('Ctrl Pts',(42.1809185638422,36.3541666734946,-24.3531646875));
#11073=CARTESIAN_POINT('Ctrl Pts',(47.5573898704234,36.1825149229327,-15.0408432190651));
#11074=CARTESIAN_POINT('Ctrl Pts',(48.5134353784344,36.0074536451604,-4.33048599679682));
#11075=CARTESIAN_POINT('',(48.5134353784344,34.7574536451604,-4.33048599679682));
#11076=CARTESIAN_POINT('',(48.5134353784344,36.0074536451604,-4.33048599679682));
#11077=CARTESIAN_POINT('',(3.46814984980029,35.8816082987783,-48.5826971030358));
#11078=CARTESIAN_POINT('Ctrl Pts',(3.46814984980029,35.8816082987783,-48.5826971030357));
#11079=CARTESIAN_POINT('Ctrl Pts',(14.6471927118254,35.6997411545207,-47.7846640967449));
#11080=CARTESIAN_POINT('Ctrl Pts',(24.3531646875,35.5208333401613,-42.1809185638422));
#11081=CARTESIAN_POINT('Ctrl Pts',(35.6555077526845,35.312500006828,-35.6555077526845));
#11082=CARTESIAN_POINT('Ctrl Pts',(42.1809185638422,35.1041666734946,-24.3531646875));
#11083=CARTESIAN_POINT('Ctrl Pts',(47.5573898704235,34.9325149229327,-15.0408432190651));
#11084=CARTESIAN_POINT('Ctrl Pts',(48.5134353784344,34.7574536451604,-4.33048599679682));
#11085=CARTESIAN_POINT('',(3.61293045337858,36.9438035983107,-48.5721446080567));
#11086=CARTESIAN_POINT('Ctrl Pts',(3.46814984980031,35.8816082987783,-48.5826971030356));
#11087=CARTESIAN_POINT('Ctrl Pts',(3.56615768657923,36.2344423378917,-48.5757006642894));
#11088=CARTESIAN_POINT('Ctrl Pts',(3.61293362241916,36.5973099952525,-48.5721446080566));
#11089=CARTESIAN_POINT('Ctrl Pts',(3.61293362241916,36.9438035983105,-48.5721446080566));
#11090=CARTESIAN_POINT('',(3.61292728433799,36.9438035983105,-48.5721446080568));
#11091=CARTESIAN_POINT('Origin',(-7.99360577730113E-14,57.8125000068276,
4.34631818602828E-14));
#11092=CARTESIAN_POINT('',(48.5725845633798,34.6293483229262,3.60701400320329));
#11093=CARTESIAN_POINT('',(1.54954344745643,33.4623411901214,48.6816745427931));
#11094=CARTESIAN_POINT('Ctrl Pts',(48.5725845633798,34.6293483229262,3.60701400320329));
#11095=CARTESIAN_POINT('Ctrl Pts',(47.7480251419552,34.4485714020251,14.7106532430575));
#11096=CARTESIAN_POINT('Ctrl Pts',(42.1809185638422,34.2708333401613,24.3531646875));
#11097=CARTESIAN_POINT('Ctrl Pts',(35.6555077526845,34.062500006828,35.6555077526845));
#11098=CARTESIAN_POINT('Ctrl Pts',(24.3531646875,33.8541666734946,42.1809185638422));
#11099=CARTESIAN_POINT('Ctrl Pts',(13.7670955736885,33.6590362432238,48.2927884163613));
#11100=CARTESIAN_POINT('Ctrl Pts',(1.54954344745643,33.4623411901214,48.6816745427932));
#11101=CARTESIAN_POINT('',(48.5725845633798,35.8793483229262,3.60701400320329));
#11102=CARTESIAN_POINT('',(48.5725845633798,34.6293483229262,3.60701400320329));
#11103=CARTESIAN_POINT('',(2.94136876951422,34.7348340040708,48.6174338169726));
#11104=CARTESIAN_POINT('Ctrl Pts',(48.5725845633798,35.8793483229262,3.60701400320329));
#11105=CARTESIAN_POINT('Ctrl Pts',(47.7480251419552,35.6985714020251,14.7106532430575));
#11106=CARTESIAN_POINT('Ctrl Pts',(42.1809185638422,35.5208333401613,24.3531646875));
#11107=CARTESIAN_POINT('Ctrl Pts',(35.6555077526845,35.312500006828,35.6555077526845));
#11108=CARTESIAN_POINT('Ctrl Pts',(24.3531646875,35.1041666734946,42.1809185638422));
#11109=CARTESIAN_POINT('Ctrl Pts',(14.4061866175215,34.9208164525749,47.9238090301676));
#11110=CARTESIAN_POINT('Ctrl Pts',(2.94136876951422,34.7348340040708,48.6174338169726));
#11111=CARTESIAN_POINT('Ctrl Pts',(2.94136876951423,34.7348340040708,48.6174338169726));
#11112=CARTESIAN_POINT('Ctrl Pts',(2.79472533668362,34.5159488958697,48.6263057869578));
#11113=CARTESIAN_POINT('Ctrl Pts',(2.62805668979196,34.3149976738954,48.6357018449976));
#11114=CARTESIAN_POINT('Ctrl Pts',(2.19334294752016,33.880330228219,48.6575995652533));
#11115=CARTESIAN_POINT('Ctrl Pts',(1.88701847015379,33.6470369515028,48.6709326729825));
#11116=CARTESIAN_POINT('Ctrl Pts',(1.54954344745642,33.4623411901214,48.6816745427931));
#11117=CARTESIAN_POINT('Ctrl Pts',(-48.706329375,58.437500006828,-1.8898197019151E-14));
#11118=CARTESIAN_POINT('Ctrl Pts',(-48.706329375,58.2291666734946,-13.0508216223155));
#11119=CARTESIAN_POINT('Ctrl Pts',(-42.1809185638422,58.0208333401613,-24.3531646875));
#11120=CARTESIAN_POINT('Ctrl Pts',(-35.6555077526845,57.812500006828,-35.6555077526845));
#11121=CARTESIAN_POINT('Ctrl Pts',(-24.3531646875,57.6041666734946,-42.1809185638422));
#11122=CARTESIAN_POINT('Ctrl Pts',(-13.0508216223155,57.3958333401613,-48.706329375));
#11123=CARTESIAN_POINT('Ctrl Pts',(1.59157945007855E-14,57.187500006828,
-48.706329375));
#11124=CARTESIAN_POINT('Ctrl Pts',(13.0508216223155,56.9791666734946,-48.706329375));
#11125=CARTESIAN_POINT('Ctrl Pts',(24.3531646875,56.7708333401613,-42.1809185638422));
#11126=CARTESIAN_POINT('Ctrl Pts',(35.6555077526845,56.562500006828,-35.6555077526845));
#11127=CARTESIAN_POINT('Ctrl Pts',(42.1809185638422,56.3541666734946,-24.3531646875));
#11128=CARTESIAN_POINT('Ctrl Pts',(48.706329375,56.1458333401613,-13.0508216223155));
#11129=CARTESIAN_POINT('Ctrl Pts',(48.706329375,55.937500006828,1.293339198242E-14));
#11130=CARTESIAN_POINT('Ctrl Pts',(48.706329375,55.7291666734946,13.0508216223155));
#11131=CARTESIAN_POINT('Ctrl Pts',(42.1809185638422,55.5208333401613,24.3531646875));
#11132=CARTESIAN_POINT('Ctrl Pts',(35.6555077526845,55.312500006828,35.6555077526845));
#11133=CARTESIAN_POINT('Ctrl Pts',(24.3531646875,55.1041666734946,42.1809185638422));
#11134=CARTESIAN_POINT('Ctrl Pts',(13.0508216223155,54.8958333401613,48.706329375));
#11135=CARTESIAN_POINT('Ctrl Pts',(-9.95098946405443E-15,54.687500006828,
48.706329375));
#11136=CARTESIAN_POINT('Ctrl Pts',(-13.0508216223155,54.4791666734946,48.706329375));
#11137=CARTESIAN_POINT('Ctrl Pts',(-24.3531646875,54.2708333401613,42.1809185638423));
#11138=CARTESIAN_POINT('Ctrl Pts',(-35.6555077526845,54.062500006828,35.6555077526845));
#11139=CARTESIAN_POINT('Ctrl Pts',(-42.1809185638422,53.8541666734946,24.3531646875));
#11140=CARTESIAN_POINT('Ctrl Pts',(-48.706329375,53.6458333401613,13.0508216223155));
#11141=CARTESIAN_POINT('Ctrl Pts',(-48.706329375,53.437500006828,-1.8898197019151E-14));
#11142=CARTESIAN_POINT('Ctrl Pts',(-48.706329375,53.2291666734946,-13.0508216223155));
#11143=CARTESIAN_POINT('Ctrl Pts',(-42.1809185638422,53.0208333401613,-24.3531646875));
#11144=CARTESIAN_POINT('Ctrl Pts',(-35.6555077526845,52.812500006828,-35.6555077526845));
#11145=CARTESIAN_POINT('Ctrl Pts',(-24.3531646875,52.6041666734946,-42.1809185638422));
#11146=CARTESIAN_POINT('Ctrl Pts',(-13.0508216223155,52.3958333401613,-48.706329375));
#11147=CARTESIAN_POINT('Ctrl Pts',(1.59157945007855E-14,52.187500006828,
-48.706329375));
#11148=CARTESIAN_POINT('Ctrl Pts',(13.0508216223155,51.9791666734946,-48.706329375));
#11149=CARTESIAN_POINT('Ctrl Pts',(24.3531646875,51.7708333401613,-42.1809185638422));
#11150=CARTESIAN_POINT('Ctrl Pts',(35.6555077526845,51.562500006828,-35.6555077526845));
#11151=CARTESIAN_POINT('Ctrl Pts',(42.1809185638422,51.3541666734946,-24.3531646875));
#11152=CARTESIAN_POINT('Ctrl Pts',(48.706329375,51.1458333401613,-13.0508216223155));
#11153=CARTESIAN_POINT('Ctrl Pts',(48.706329375,50.937500006828,1.293339198242E-14));
#11154=CARTESIAN_POINT('Ctrl Pts',(48.706329375,50.7291666734946,13.0508216223155));
#11155=CARTESIAN_POINT('Ctrl Pts',(42.1809185638422,50.5208333401613,24.3531646875));
#11156=CARTESIAN_POINT('Ctrl Pts',(35.6555077526845,50.312500006828,35.6555077526845));
#11157=CARTESIAN_POINT('Ctrl Pts',(24.3531646875,50.1041666734946,42.1809185638422));
#11158=CARTESIAN_POINT('Ctrl Pts',(13.0508216223155,49.8958333401613,48.706329375));
#11159=CARTESIAN_POINT('Ctrl Pts',(-9.95098946405443E-15,49.687500006828,
48.706329375));
#11160=CARTESIAN_POINT('Ctrl Pts',(-13.0508216223155,49.4791666734946,48.706329375));
#11161=CARTESIAN_POINT('Ctrl Pts',(-24.3531646875,49.2708333401613,42.1809185638423));
#11162=CARTESIAN_POINT('Ctrl Pts',(-35.6555077526845,49.062500006828,35.6555077526845));
#11163=CARTESIAN_POINT('Ctrl Pts',(-42.1809185638422,48.8541666734946,24.3531646875));
#11164=CARTESIAN_POINT('Ctrl Pts',(-48.706329375,48.6458333401613,13.0508216223155));
#11165=CARTESIAN_POINT('Ctrl Pts',(-48.706329375,48.437500006828,-1.8898197019151E-14));
#11166=CARTESIAN_POINT('Ctrl Pts',(-48.706329375,48.2291666734946,-13.0508216223155));
#11167=CARTESIAN_POINT('Ctrl Pts',(-42.1809185638422,48.0208333401613,-24.3531646875));
#11168=CARTESIAN_POINT('Ctrl Pts',(-35.6555077526845,47.812500006828,-35.6555077526845));
#11169=CARTESIAN_POINT('Ctrl Pts',(-24.3531646875,47.6041666734946,-42.1809185638422));
#11170=CARTESIAN_POINT('Ctrl Pts',(-13.0508216223155,47.3958333401613,-48.706329375));
#11171=CARTESIAN_POINT('Ctrl Pts',(1.59157945007855E-14,47.187500006828,
-48.706329375));
#11172=CARTESIAN_POINT('Ctrl Pts',(13.0508216223155,46.9791666734946,-48.706329375));
#11173=CARTESIAN_POINT('Ctrl Pts',(24.3531646875,46.7708333401613,-42.1809185638422));
#11174=CARTESIAN_POINT('Ctrl Pts',(35.6555077526845,46.562500006828,-35.6555077526845));
#11175=CARTESIAN_POINT('Ctrl Pts',(42.1809185638422,46.3541666734946,-24.3531646875));
#11176=CARTESIAN_POINT('Ctrl Pts',(48.706329375,46.1458333401613,-13.0508216223155));
#11177=CARTESIAN_POINT('Ctrl Pts',(48.706329375,45.937500006828,1.293339198242E-14));
#11178=CARTESIAN_POINT('Ctrl Pts',(48.706329375,45.7291666734946,13.0508216223155));
#11179=CARTESIAN_POINT('Ctrl Pts',(42.1809185638422,45.5208333401613,24.3531646875));
#11180=CARTESIAN_POINT('Ctrl Pts',(35.6555077526845,45.312500006828,35.6555077526845));
#11181=CARTESIAN_POINT('Ctrl Pts',(24.3531646875,45.1041666734946,42.1809185638422));
#11182=CARTESIAN_POINT('Ctrl Pts',(13.0508216223155,44.8958333401613,48.706329375));
#11183=CARTESIAN_POINT('Ctrl Pts',(-9.95098946405443E-15,44.687500006828,
48.706329375));
#11184=CARTESIAN_POINT('Ctrl Pts',(-13.0508216223155,44.4791666734946,48.706329375));
#11185=CARTESIAN_POINT('Ctrl Pts',(-24.3531646875,44.2708333401613,42.1809185638423));
#11186=CARTESIAN_POINT('Ctrl Pts',(-35.6555077526845,44.062500006828,35.6555077526845));
#11187=CARTESIAN_POINT('Ctrl Pts',(-42.1809185638422,43.8541666734946,24.3531646875));
#11188=CARTESIAN_POINT('Ctrl Pts',(-48.706329375,43.6458333401613,13.0508216223155));
#11189=CARTESIAN_POINT('Ctrl Pts',(-48.706329375,43.437500006828,-1.8898197019151E-14));
#11190=CARTESIAN_POINT('Ctrl Pts',(-48.706329375,43.2291666734946,-13.0508216223155));
#11191=CARTESIAN_POINT('Ctrl Pts',(-42.1809185638422,43.0208333401613,-24.3531646875));
#11192=CARTESIAN_POINT('Ctrl Pts',(-35.6555077526845,42.812500006828,-35.6555077526845));
#11193=CARTESIAN_POINT('Ctrl Pts',(-24.3531646875,42.6041666734946,-42.1809185638422));
#11194=CARTESIAN_POINT('Ctrl Pts',(-13.0508216223155,42.3958333401613,-48.706329375));
#11195=CARTESIAN_POINT('Ctrl Pts',(1.59157945007855E-14,42.187500006828,
-48.706329375));
#11196=CARTESIAN_POINT('Ctrl Pts',(13.0508216223155,41.9791666734946,-48.706329375));
#11197=CARTESIAN_POINT('Ctrl Pts',(24.3531646875,41.7708333401613,-42.1809185638422));
#11198=CARTESIAN_POINT('Ctrl Pts',(35.6555077526845,41.562500006828,-35.6555077526845));
#11199=CARTESIAN_POINT('Ctrl Pts',(42.1809185638422,41.3541666734946,-24.3531646875));
#11200=CARTESIAN_POINT('Ctrl Pts',(48.706329375,41.1458333401613,-13.0508216223155));
#11201=CARTESIAN_POINT('Ctrl Pts',(48.706329375,40.937500006828,1.293339198242E-14));
#11202=CARTESIAN_POINT('Ctrl Pts',(48.706329375,40.7291666734946,13.0508216223155));
#11203=CARTESIAN_POINT('Ctrl Pts',(42.1809185638422,40.5208333401613,24.3531646875));
#11204=CARTESIAN_POINT('Ctrl Pts',(35.6555077526845,40.312500006828,35.6555077526845));
#11205=CARTESIAN_POINT('Ctrl Pts',(24.3531646875,40.1041666734946,42.1809185638422));
#11206=CARTESIAN_POINT('Ctrl Pts',(13.0508216223155,39.8958333401613,48.706329375));
#11207=CARTESIAN_POINT('Ctrl Pts',(-9.95098946405443E-15,39.687500006828,
48.706329375));
#11208=CARTESIAN_POINT('Ctrl Pts',(-13.0508216223155,39.4791666734946,48.706329375));
#11209=CARTESIAN_POINT('Ctrl Pts',(-24.3531646875,39.2708333401613,42.1809185638423));
#11210=CARTESIAN_POINT('Ctrl Pts',(-35.6555077526845,39.062500006828,35.6555077526845));
#11211=CARTESIAN_POINT('Ctrl Pts',(-42.1809185638422,38.8541666734946,24.3531646875));
#11212=CARTESIAN_POINT('Ctrl Pts',(-48.706329375,38.6458333401613,13.0508216223155));
#11213=CARTESIAN_POINT('Ctrl Pts',(-48.706329375,38.437500006828,-1.8898197019151E-14));
#11214=CARTESIAN_POINT('Ctrl Pts',(-48.706329375,38.2291666734946,-13.0508216223155));
#11215=CARTESIAN_POINT('Ctrl Pts',(-42.1809185638422,38.0208333401613,-24.3531646875));
#11216=CARTESIAN_POINT('Ctrl Pts',(-35.6555077526845,37.812500006828,-35.6555077526845));
#11217=CARTESIAN_POINT('Ctrl Pts',(-24.3531646875,37.6041666734946,-42.1809185638422));
#11218=CARTESIAN_POINT('Ctrl Pts',(-13.0508216223155,37.3958333401613,-48.706329375));
#11219=CARTESIAN_POINT('Ctrl Pts',(1.59157945007855E-14,37.187500006828,
-48.706329375));
#11220=CARTESIAN_POINT('Ctrl Pts',(13.0508216223155,36.9791666734946,-48.706329375));
#11221=CARTESIAN_POINT('Ctrl Pts',(24.3531646875,36.7708333401613,-42.1809185638422));
#11222=CARTESIAN_POINT('Ctrl Pts',(35.6555077526845,36.562500006828,-35.6555077526845));
#11223=CARTESIAN_POINT('Ctrl Pts',(42.1809185638422,36.3541666734946,-24.3531646875));
#11224=CARTESIAN_POINT('Ctrl Pts',(48.706329375,36.1458333401613,-13.0508216223155));
#11225=CARTESIAN_POINT('Ctrl Pts',(48.706329375,35.937500006828,1.293339198242E-14));
#11226=CARTESIAN_POINT('Ctrl Pts',(48.706329375,35.7291666734946,13.0508216223155));
#11227=CARTESIAN_POINT('Ctrl Pts',(42.1809185638422,35.5208333401613,24.3531646875));
#11228=CARTESIAN_POINT('Ctrl Pts',(35.6555077526845,35.312500006828,35.6555077526845));
#11229=CARTESIAN_POINT('Ctrl Pts',(24.3531646875,35.1041666734946,42.1809185638422));
#11230=CARTESIAN_POINT('Ctrl Pts',(13.0508216223155,34.8958333401613,48.706329375));
#11231=CARTESIAN_POINT('Ctrl Pts',(-9.95098946405443E-15,34.687500006828,
48.706329375));
#11232=CARTESIAN_POINT('Ctrl Pts',(-13.0508216223155,34.4791666734946,48.706329375));
#11233=CARTESIAN_POINT('Ctrl Pts',(-24.3531646875,34.2708333401613,42.1809185638423));
#11234=CARTESIAN_POINT('Ctrl Pts',(-35.6555077526845,34.062500006828,35.6555077526845));
#11235=CARTESIAN_POINT('Ctrl Pts',(-42.1809185638422,33.8541666734946,24.3531646875));
#11236=CARTESIAN_POINT('Ctrl Pts',(-48.706329375,33.6458333401613,13.0508216223155));
#11237=CARTESIAN_POINT('Ctrl Pts',(-48.706329375,33.437500006828,-1.8898197019151E-14));
#11238=CARTESIAN_POINT('Ctrl Pts',(-48.706329375,33.2291666734946,-13.0508216223155));
#11239=CARTESIAN_POINT('Ctrl Pts',(-42.1809185638422,33.0208333401613,-24.3531646875));
#11240=CARTESIAN_POINT('Ctrl Pts',(-35.6555077526845,32.812500006828,-35.6555077526845));
#11241=CARTESIAN_POINT('Ctrl Pts',(-24.3531646875,32.6041666734946,-42.1809185638422));
#11242=CARTESIAN_POINT('Ctrl Pts',(-13.0508216223155,32.3958333401613,-48.706329375));
#11243=CARTESIAN_POINT('Ctrl Pts',(1.59157945007855E-14,32.187500006828,
-48.706329375));
#11244=CARTESIAN_POINT('Ctrl Pts',(13.0508216223155,31.9791666734946,-48.706329375));
#11245=CARTESIAN_POINT('Ctrl Pts',(24.3531646875,31.7708333401613,-42.1809185638422));
#11246=CARTESIAN_POINT('Ctrl Pts',(35.6555077526845,31.562500006828,-35.6555077526845));
#11247=CARTESIAN_POINT('Ctrl Pts',(42.1809185638422,31.3541666734946,-24.3531646875));
#11248=CARTESIAN_POINT('Ctrl Pts',(48.706329375,31.1458333401613,-13.0508216223155));
#11249=CARTESIAN_POINT('Ctrl Pts',(48.706329375,30.937500006828,1.293339198242E-14));
#11250=CARTESIAN_POINT('Ctrl Pts',(48.706329375,30.7291666734946,13.0508216223155));
#11251=CARTESIAN_POINT('Ctrl Pts',(42.1809185638422,30.5208333401613,24.3531646875));
#11252=CARTESIAN_POINT('Ctrl Pts',(35.6555077526845,30.312500006828,35.6555077526845));
#11253=CARTESIAN_POINT('Ctrl Pts',(24.3531646875,30.1041666734946,42.1809185638422));
#11254=CARTESIAN_POINT('Ctrl Pts',(13.0508216223155,29.8958333401613,48.706329375));
#11255=CARTESIAN_POINT('Ctrl Pts',(-9.95098946405443E-15,29.687500006828,
48.706329375));
#11256=CARTESIAN_POINT('Ctrl Pts',(-13.0508216223155,29.4791666734946,48.706329375));
#11257=CARTESIAN_POINT('Ctrl Pts',(-24.3531646875,29.2708333401613,42.1809185638423));
#11258=CARTESIAN_POINT('Ctrl Pts',(-35.6555077526845,29.062500006828,35.6555077526845));
#11259=CARTESIAN_POINT('Ctrl Pts',(-42.1809185638422,28.8541666734946,24.3531646875));
#11260=CARTESIAN_POINT('Ctrl Pts',(-48.706329375,28.6458333401613,13.0508216223155));
#11261=CARTESIAN_POINT('Ctrl Pts',(-48.706329375,28.437500006828,-1.8898197019151E-14));
#11262=CARTESIAN_POINT('Ctrl Pts',(-46.,60.,0.));
#11263=CARTESIAN_POINT('Ctrl Pts',(-46.,59.7916666666667,-12.3256628518316));
#11264=CARTESIAN_POINT('Ctrl Pts',(-39.8371685740842,59.5833333333333,-23.));
#11265=CARTESIAN_POINT('Ctrl Pts',(-33.6743371481684,59.375,-33.6743371481684));
#11266=CARTESIAN_POINT('Ctrl Pts',(-23.,59.1666666666667,-39.8371685740842));
#11267=CARTESIAN_POINT('Ctrl Pts',(-12.3256628518317,58.9583333333333,-46.));
#11268=CARTESIAN_POINT('Ctrl Pts',(-2.81668763803891E-15,58.75,-46.));
#11269=CARTESIAN_POINT('Ctrl Pts',(12.3256628518316,58.5416666666667,-46.));
#11270=CARTESIAN_POINT('Ctrl Pts',(23.,58.3333333333333,-39.8371685740842));
#11271=CARTESIAN_POINT('Ctrl Pts',(33.6743371481683,58.125,-33.6743371481684));
#11272=CARTESIAN_POINT('Ctrl Pts',(39.8371685740842,57.9166666666667,-23.));
#11273=CARTESIAN_POINT('Ctrl Pts',(46.,57.7083333333333,-12.3256628518317));
#11274=CARTESIAN_POINT('Ctrl Pts',(46.,57.5,-5.63337527607782E-15));
#11275=CARTESIAN_POINT('Ctrl Pts',(46.,57.2916666666667,12.3256628518316));
#11276=CARTESIAN_POINT('Ctrl Pts',(39.8371685740842,57.0833333333333,23.));
#11277=CARTESIAN_POINT('Ctrl Pts',(33.6743371481684,56.875,33.6743371481683));
#11278=CARTESIAN_POINT('Ctrl Pts',(23.,56.6666666666667,39.8371685740842));
#11279=CARTESIAN_POINT('Ctrl Pts',(12.3256628518317,56.4583333333333,46.));
#11280=CARTESIAN_POINT('Ctrl Pts',(8.45006291411674E-15,56.25,46.));
#11281=CARTESIAN_POINT('Ctrl Pts',(-12.3256628518316,56.0416666666667,46.));
#11282=CARTESIAN_POINT('Ctrl Pts',(-23.,55.8333333333333,39.8371685740842));
#11283=CARTESIAN_POINT('Ctrl Pts',(-33.6743371481683,55.625,33.6743371481684));
#11284=CARTESIAN_POINT('Ctrl Pts',(-39.8371685740842,55.4166666666667,23.));
#11285=CARTESIAN_POINT('Ctrl Pts',(-46.,55.2083333333333,12.3256628518317));
#11286=CARTESIAN_POINT('Ctrl Pts',(-46.,55.,0.));
#11287=CARTESIAN_POINT('Ctrl Pts',(-46.,54.7916666666667,-12.3256628518316));
#11288=CARTESIAN_POINT('Ctrl Pts',(-39.8371685740842,54.5833333333333,-23.));
#11289=CARTESIAN_POINT('Ctrl Pts',(-33.6743371481684,54.375,-33.6743371481684));
#11290=CARTESIAN_POINT('Ctrl Pts',(-23.,54.1666666666667,-39.8371685740842));
#11291=CARTESIAN_POINT('Ctrl Pts',(-12.3256628518317,53.9583333333333,-46.));
#11292=CARTESIAN_POINT('Ctrl Pts',(-2.81668763803891E-15,53.75,-46.));
#11293=CARTESIAN_POINT('Ctrl Pts',(12.3256628518316,53.5416666666667,-46.));
#11294=CARTESIAN_POINT('Ctrl Pts',(23.,53.3333333333333,-39.8371685740842));
#11295=CARTESIAN_POINT('Ctrl Pts',(33.6743371481683,53.125,-33.6743371481684));
#11296=CARTESIAN_POINT('Ctrl Pts',(39.8371685740842,52.9166666666667,-23.));
#11297=CARTESIAN_POINT('Ctrl Pts',(46.,52.7083333333333,-12.3256628518317));
#11298=CARTESIAN_POINT('Ctrl Pts',(46.,52.5,-5.63337527607782E-15));
#11299=CARTESIAN_POINT('Ctrl Pts',(46.,52.2916666666667,12.3256628518316));
#11300=CARTESIAN_POINT('Ctrl Pts',(39.8371685740842,52.0833333333333,23.));
#11301=CARTESIAN_POINT('Ctrl Pts',(33.6743371481684,51.875,33.6743371481683));
#11302=CARTESIAN_POINT('Ctrl Pts',(23.,51.6666666666667,39.8371685740842));
#11303=CARTESIAN_POINT('Ctrl Pts',(12.3256628518317,51.4583333333333,46.));
#11304=CARTESIAN_POINT('Ctrl Pts',(8.45006291411674E-15,51.25,46.));
#11305=CARTESIAN_POINT('Ctrl Pts',(-12.3256628518316,51.0416666666667,46.));
#11306=CARTESIAN_POINT('Ctrl Pts',(-23.,50.8333333333333,39.8371685740842));
#11307=CARTESIAN_POINT('Ctrl Pts',(-33.6743371481683,50.625,33.6743371481684));
#11308=CARTESIAN_POINT('Ctrl Pts',(-39.8371685740842,50.4166666666667,23.));
#11309=CARTESIAN_POINT('Ctrl Pts',(-46.,50.2083333333333,12.3256628518317));
#11310=CARTESIAN_POINT('Ctrl Pts',(-46.,50.,0.));
#11311=CARTESIAN_POINT('Ctrl Pts',(-46.,49.7916666666667,-12.3256628518316));
#11312=CARTESIAN_POINT('Ctrl Pts',(-39.8371685740842,49.5833333333333,-23.));
#11313=CARTESIAN_POINT('Ctrl Pts',(-33.6743371481684,49.375,-33.6743371481684));
#11314=CARTESIAN_POINT('Ctrl Pts',(-23.,49.1666666666667,-39.8371685740842));
#11315=CARTESIAN_POINT('Ctrl Pts',(-12.3256628518317,48.9583333333333,-46.));
#11316=CARTESIAN_POINT('Ctrl Pts',(-2.81668763803891E-15,48.75,-46.));
#11317=CARTESIAN_POINT('Ctrl Pts',(12.3256628518316,48.5416666666667,-46.));
#11318=CARTESIAN_POINT('Ctrl Pts',(23.,48.3333333333333,-39.8371685740842));
#11319=CARTESIAN_POINT('Ctrl Pts',(33.6743371481683,48.125,-33.6743371481684));
#11320=CARTESIAN_POINT('Ctrl Pts',(39.8371685740842,47.9166666666667,-23.));
#11321=CARTESIAN_POINT('Ctrl Pts',(46.,47.7083333333333,-12.3256628518317));
#11322=CARTESIAN_POINT('Ctrl Pts',(46.,47.5,-5.63337527607782E-15));
#11323=CARTESIAN_POINT('Ctrl Pts',(46.,47.2916666666667,12.3256628518316));
#11324=CARTESIAN_POINT('Ctrl Pts',(39.8371685740842,47.0833333333333,23.));
#11325=CARTESIAN_POINT('Ctrl Pts',(33.6743371481684,46.875,33.6743371481683));
#11326=CARTESIAN_POINT('Ctrl Pts',(23.,46.6666666666667,39.8371685740842));
#11327=CARTESIAN_POINT('Ctrl Pts',(12.3256628518317,46.4583333333333,46.));
#11328=CARTESIAN_POINT('Ctrl Pts',(8.45006291411674E-15,46.25,46.));
#11329=CARTESIAN_POINT('Ctrl Pts',(-12.3256628518316,46.0416666666667,46.));
#11330=CARTESIAN_POINT('Ctrl Pts',(-23.,45.8333333333333,39.8371685740842));
#11331=CARTESIAN_POINT('Ctrl Pts',(-33.6743371481683,45.625,33.6743371481684));
#11332=CARTESIAN_POINT('Ctrl Pts',(-39.8371685740842,45.4166666666667,23.));
#11333=CARTESIAN_POINT('Ctrl Pts',(-46.,45.2083333333333,12.3256628518317));
#11334=CARTESIAN_POINT('Ctrl Pts',(-46.,45.,0.));
#11335=CARTESIAN_POINT('Ctrl Pts',(-46.,44.7916666666667,-12.3256628518316));
#11336=CARTESIAN_POINT('Ctrl Pts',(-39.8371685740842,44.5833333333333,-23.));
#11337=CARTESIAN_POINT('Ctrl Pts',(-33.6743371481684,44.375,-33.6743371481684));
#11338=CARTESIAN_POINT('Ctrl Pts',(-23.,44.1666666666667,-39.8371685740842));
#11339=CARTESIAN_POINT('Ctrl Pts',(-12.3256628518317,43.9583333333333,-46.));
#11340=CARTESIAN_POINT('Ctrl Pts',(-2.81668763803891E-15,43.75,-46.));
#11341=CARTESIAN_POINT('Ctrl Pts',(12.3256628518316,43.5416666666667,-46.));
#11342=CARTESIAN_POINT('Ctrl Pts',(23.,43.3333333333333,-39.8371685740842));
#11343=CARTESIAN_POINT('Ctrl Pts',(33.6743371481683,43.125,-33.6743371481684));
#11344=CARTESIAN_POINT('Ctrl Pts',(39.8371685740842,42.9166666666667,-23.));
#11345=CARTESIAN_POINT('Ctrl Pts',(46.,42.7083333333333,-12.3256628518317));
#11346=CARTESIAN_POINT('Ctrl Pts',(46.,42.5,-5.63337527607782E-15));
#11347=CARTESIAN_POINT('Ctrl Pts',(46.,42.2916666666667,12.3256628518316));
#11348=CARTESIAN_POINT('Ctrl Pts',(39.8371685740842,42.0833333333333,23.));
#11349=CARTESIAN_POINT('Ctrl Pts',(33.6743371481684,41.875,33.6743371481683));
#11350=CARTESIAN_POINT('Ctrl Pts',(23.,41.6666666666667,39.8371685740842));
#11351=CARTESIAN_POINT('Ctrl Pts',(12.3256628518317,41.4583333333333,46.));
#11352=CARTESIAN_POINT('Ctrl Pts',(8.45006291411674E-15,41.25,46.));
#11353=CARTESIAN_POINT('Ctrl Pts',(-12.3256628518316,41.0416666666667,46.));
#11354=CARTESIAN_POINT('Ctrl Pts',(-23.,40.8333333333333,39.8371685740842));
#11355=CARTESIAN_POINT('Ctrl Pts',(-33.6743371481683,40.625,33.6743371481684));
#11356=CARTESIAN_POINT('Ctrl Pts',(-39.8371685740842,40.4166666666667,23.));
#11357=CARTESIAN_POINT('Ctrl Pts',(-46.,40.2083333333333,12.3256628518317));
#11358=CARTESIAN_POINT('Ctrl Pts',(-46.,40.,0.));
#11359=CARTESIAN_POINT('Ctrl Pts',(-46.,39.7916666666667,-12.3256628518316));
#11360=CARTESIAN_POINT('Ctrl Pts',(-39.8371685740842,39.5833333333333,-23.));
#11361=CARTESIAN_POINT('Ctrl Pts',(-33.6743371481684,39.375,-33.6743371481684));
#11362=CARTESIAN_POINT('Ctrl Pts',(-23.,39.1666666666667,-39.8371685740842));
#11363=CARTESIAN_POINT('Ctrl Pts',(-12.3256628518317,38.9583333333333,-46.));
#11364=CARTESIAN_POINT('Ctrl Pts',(-2.81668763803891E-15,38.75,-46.));
#11365=CARTESIAN_POINT('Ctrl Pts',(12.3256628518316,38.5416666666667,-46.));
#11366=CARTESIAN_POINT('Ctrl Pts',(23.,38.3333333333333,-39.8371685740842));
#11367=CARTESIAN_POINT('Ctrl Pts',(33.6743371481683,38.125,-33.6743371481684));
#11368=CARTESIAN_POINT('Ctrl Pts',(39.8371685740842,37.9166666666667,-23.));
#11369=CARTESIAN_POINT('Ctrl Pts',(46.,37.7083333333333,-12.3256628518317));
#11370=CARTESIAN_POINT('Ctrl Pts',(46.,37.5,-5.63337527607782E-15));
#11371=CARTESIAN_POINT('Ctrl Pts',(46.,37.2916666666667,12.3256628518316));
#11372=CARTESIAN_POINT('Ctrl Pts',(39.8371685740842,37.0833333333333,23.));
#11373=CARTESIAN_POINT('Ctrl Pts',(33.6743371481684,36.875,33.6743371481683));
#11374=CARTESIAN_POINT('Ctrl Pts',(23.,36.6666666666667,39.8371685740842));
#11375=CARTESIAN_POINT('Ctrl Pts',(12.3256628518317,36.4583333333333,46.));
#11376=CARTESIAN_POINT('Ctrl Pts',(8.45006291411674E-15,36.25,46.));
#11377=CARTESIAN_POINT('Ctrl Pts',(-12.3256628518316,36.0416666666667,46.));
#11378=CARTESIAN_POINT('Ctrl Pts',(-23.,35.8333333333333,39.8371685740842));
#11379=CARTESIAN_POINT('Ctrl Pts',(-33.6743371481683,35.625,33.6743371481684));
#11380=CARTESIAN_POINT('Ctrl Pts',(-39.8371685740842,35.4166666666667,23.));
#11381=CARTESIAN_POINT('Ctrl Pts',(-46.,35.2083333333333,12.3256628518317));
#11382=CARTESIAN_POINT('Ctrl Pts',(-46.,35.,0.));
#11383=CARTESIAN_POINT('Ctrl Pts',(-46.,34.7916666666667,-12.3256628518316));
#11384=CARTESIAN_POINT('Ctrl Pts',(-39.8371685740842,34.5833333333333,-23.));
#11385=CARTESIAN_POINT('Ctrl Pts',(-33.6743371481684,34.375,-33.6743371481684));
#11386=CARTESIAN_POINT('Ctrl Pts',(-23.,34.1666666666667,-39.8371685740842));
#11387=CARTESIAN_POINT('Ctrl Pts',(-12.3256628518317,33.9583333333333,-46.));
#11388=CARTESIAN_POINT('Ctrl Pts',(-2.81668763803891E-15,33.75,-46.));
#11389=CARTESIAN_POINT('Ctrl Pts',(12.3256628518316,33.5416666666667,-46.));
#11390=CARTESIAN_POINT('Ctrl Pts',(23.,33.3333333333333,-39.8371685740842));
#11391=CARTESIAN_POINT('Ctrl Pts',(33.6743371481683,33.125,-33.6743371481684));
#11392=CARTESIAN_POINT('Ctrl Pts',(39.8371685740842,32.9166666666667,-23.));
#11393=CARTESIAN_POINT('Ctrl Pts',(46.,32.7083333333333,-12.3256628518317));
#11394=CARTESIAN_POINT('Ctrl Pts',(46.,32.5,-5.63337527607782E-15));
#11395=CARTESIAN_POINT('Ctrl Pts',(46.,32.2916666666667,12.3256628518316));
#11396=CARTESIAN_POINT('Ctrl Pts',(39.8371685740842,32.0833333333333,23.));
#11397=CARTESIAN_POINT('Ctrl Pts',(33.6743371481684,31.875,33.6743371481683));
#11398=CARTESIAN_POINT('Ctrl Pts',(23.,31.6666666666667,39.8371685740842));
#11399=CARTESIAN_POINT('Ctrl Pts',(12.3256628518317,31.4583333333333,46.));
#11400=CARTESIAN_POINT('Ctrl Pts',(8.45006291411674E-15,31.25,46.));
#11401=CARTESIAN_POINT('Ctrl Pts',(-12.3256628518316,31.0416666666667,46.));
#11402=CARTESIAN_POINT('Ctrl Pts',(-23.,30.8333333333333,39.8371685740842));
#11403=CARTESIAN_POINT('Ctrl Pts',(-33.6743371481683,30.625,33.6743371481684));
#11404=CARTESIAN_POINT('Ctrl Pts',(-39.8371685740842,30.4166666666667,23.));
#11405=CARTESIAN_POINT('Ctrl Pts',(-46.,30.2083333333333,12.3256628518317));
#11406=CARTESIAN_POINT('Ctrl Pts',(-46.,30.,0.));
#11407=CARTESIAN_POINT('',(15.5677347613557,57.,-46.0186009836189));
#11408=CARTESIAN_POINT('',(46.79170203032,56.9999999999858,-4.33048599679673));
#11409=CARTESIAN_POINT('Ctrl Pts',(15.5677347613557,57.,-46.0186009836189));
#11410=CARTESIAN_POINT('Ctrl Pts',(17.7310349698886,57.,-45.2170526223414));
#11411=CARTESIAN_POINT('Ctrl Pts',(19.834567405171,57.0000000000088,-44.2626483761178));
#11412=CARTESIAN_POINT('Ctrl Pts',(23.9079865381294,57.0000000000088,-42.0529745645465));
#11413=CARTESIAN_POINT('Ctrl Pts',(25.8779679347109,57.,-40.7943833295357));
#11414=CARTESIAN_POINT('Ctrl Pts',(31.3891578561493,57.,-36.6723214087039));
#11415=CARTESIAN_POINT('Ctrl Pts',(34.6227678874526,57.,-33.4466510749012));
#11416=CARTESIAN_POINT('Ctrl Pts',(40.1411508117922,57.,-26.1061863972564));
#11417=CARTESIAN_POINT('Ctrl Pts',(42.3917117517447,57.,-21.991753538455));
#11418=CARTESIAN_POINT('Ctrl Pts',(45.5641231823138,57.,-13.3433502223045));
#11419=CARTESIAN_POINT('Ctrl Pts',(46.5051362525069,57.,-8.86952477496529));
#11420=CARTESIAN_POINT('Ctrl Pts',(46.7917020302955,57.,-4.33048599679518));
#11421=CARTESIAN_POINT('Ctrl Pts',(46.79170203032,56.9999999999858,-4.33048599679673));
#11422=CARTESIAN_POINT('Ctrl Pts',(46.9229272270402,56.92435531248,-4.33048599679673));
#11423=CARTESIAN_POINT('Ctrl Pts',(47.0541520004637,56.8487098906525,-4.33048599679673));
#11424=CARTESIAN_POINT('Ctrl Pts',(47.6280672732221,56.5178683162597,-4.33048599679673));
#11425=CARTESIAN_POINT('Ctrl Pts',(48.0707534890442,56.2626647328764,-4.33048599679674));
#11426=CARTESIAN_POINT('Ctrl Pts',(48.5134353784344,56.0074536451604,-4.33048599679673));
#11427=CARTESIAN_POINT('',(3.612927284338,57.2017412484791,-48.4459777332189));
#11428=CARTESIAN_POINT('',(3.61292728433799,57.1292520480092,-48.5721450795008));
#11429=CARTESIAN_POINT('Origin',(-0.00341856678684749,57.0518082227792,
0.0127587930744433));
#11430=CARTESIAN_POINT('Ctrl Pts',(-48.706329375,58.437500006828,-1.8898197019151E-14));
#11431=CARTESIAN_POINT('Ctrl Pts',(-48.706329375,58.2291666734946,-13.0508216223155));
#11432=CARTESIAN_POINT('Ctrl Pts',(-42.1809185638422,58.0208333401613,-24.3531646875));
#11433=CARTESIAN_POINT('Ctrl Pts',(-35.6555077526845,57.812500006828,-35.6555077526845));
#11434=CARTESIAN_POINT('Ctrl Pts',(-24.3531646875,57.6041666734946,-42.1809185638422));
#11435=CARTESIAN_POINT('Ctrl Pts',(-13.0508216223155,57.3958333401613,-48.706329375));
#11436=CARTESIAN_POINT('Ctrl Pts',(1.59157945007855E-14,57.187500006828,
-48.706329375));
#11437=CARTESIAN_POINT('Ctrl Pts',(13.0508216223155,56.9791666734946,-48.706329375));
#11438=CARTESIAN_POINT('Ctrl Pts',(24.3531646875,56.7708333401613,-42.1809185638422));
#11439=CARTESIAN_POINT('Ctrl Pts',(35.6555077526845,56.562500006828,-35.6555077526845));
#11440=CARTESIAN_POINT('Ctrl Pts',(42.1809185638422,56.3541666734946,-24.3531646875));
#11441=CARTESIAN_POINT('Ctrl Pts',(48.706329375,56.1458333401613,-13.0508216223155));
#11442=CARTESIAN_POINT('Ctrl Pts',(48.706329375,55.937500006828,1.293339198242E-14));
#11443=CARTESIAN_POINT('Ctrl Pts',(48.706329375,55.7291666734946,13.0508216223155));
#11444=CARTESIAN_POINT('Ctrl Pts',(42.1809185638422,55.5208333401613,24.3531646875));
#11445=CARTESIAN_POINT('Ctrl Pts',(35.6555077526845,55.312500006828,35.6555077526845));
#11446=CARTESIAN_POINT('Ctrl Pts',(24.3531646875,55.1041666734946,42.1809185638422));
#11447=CARTESIAN_POINT('Ctrl Pts',(13.0508216223155,54.8958333401613,48.706329375));
#11448=CARTESIAN_POINT('Ctrl Pts',(-9.95098946405443E-15,54.687500006828,
48.706329375));
#11449=CARTESIAN_POINT('Ctrl Pts',(-13.0508216223155,54.4791666734946,48.706329375));
#11450=CARTESIAN_POINT('Ctrl Pts',(-24.3531646875,54.2708333401613,42.1809185638423));
#11451=CARTESIAN_POINT('Ctrl Pts',(-35.6555077526845,54.062500006828,35.6555077526845));
#11452=CARTESIAN_POINT('Ctrl Pts',(-42.1809185638422,53.8541666734946,24.3531646875));
#11453=CARTESIAN_POINT('Ctrl Pts',(-48.706329375,53.6458333401613,13.0508216223155));
#11454=CARTESIAN_POINT('Ctrl Pts',(-48.706329375,53.437500006828,-1.8898197019151E-14));
#11455=CARTESIAN_POINT('Ctrl Pts',(-48.706329375,53.2291666734946,-13.0508216223155));
#11456=CARTESIAN_POINT('Ctrl Pts',(-42.1809185638422,53.0208333401613,-24.3531646875));
#11457=CARTESIAN_POINT('Ctrl Pts',(-35.6555077526845,52.812500006828,-35.6555077526845));
#11458=CARTESIAN_POINT('Ctrl Pts',(-24.3531646875,52.6041666734946,-42.1809185638422));
#11459=CARTESIAN_POINT('Ctrl Pts',(-13.0508216223155,52.3958333401613,-48.706329375));
#11460=CARTESIAN_POINT('Ctrl Pts',(1.59157945007855E-14,52.187500006828,
-48.706329375));
#11461=CARTESIAN_POINT('Ctrl Pts',(13.0508216223155,51.9791666734946,-48.706329375));
#11462=CARTESIAN_POINT('Ctrl Pts',(24.3531646875,51.7708333401613,-42.1809185638422));
#11463=CARTESIAN_POINT('Ctrl Pts',(35.6555077526845,51.562500006828,-35.6555077526845));
#11464=CARTESIAN_POINT('Ctrl Pts',(42.1809185638422,51.3541666734946,-24.3531646875));
#11465=CARTESIAN_POINT('Ctrl Pts',(48.706329375,51.1458333401613,-13.0508216223155));
#11466=CARTESIAN_POINT('Ctrl Pts',(48.706329375,50.937500006828,1.293339198242E-14));
#11467=CARTESIAN_POINT('Ctrl Pts',(48.706329375,50.7291666734946,13.0508216223155));
#11468=CARTESIAN_POINT('Ctrl Pts',(42.1809185638422,50.5208333401613,24.3531646875));
#11469=CARTESIAN_POINT('Ctrl Pts',(35.6555077526845,50.312500006828,35.6555077526845));
#11470=CARTESIAN_POINT('Ctrl Pts',(24.3531646875,50.1041666734946,42.1809185638422));
#11471=CARTESIAN_POINT('Ctrl Pts',(13.0508216223155,49.8958333401613,48.706329375));
#11472=CARTESIAN_POINT('Ctrl Pts',(-9.95098946405443E-15,49.687500006828,
48.706329375));
#11473=CARTESIAN_POINT('Ctrl Pts',(-13.0508216223155,49.4791666734946,48.706329375));
#11474=CARTESIAN_POINT('Ctrl Pts',(-24.3531646875,49.2708333401613,42.1809185638423));
#11475=CARTESIAN_POINT('Ctrl Pts',(-35.6555077526845,49.062500006828,35.6555077526845));
#11476=CARTESIAN_POINT('Ctrl Pts',(-42.1809185638422,48.8541666734946,24.3531646875));
#11477=CARTESIAN_POINT('Ctrl Pts',(-48.706329375,48.6458333401613,13.0508216223155));
#11478=CARTESIAN_POINT('Ctrl Pts',(-48.706329375,48.437500006828,-1.8898197019151E-14));
#11479=CARTESIAN_POINT('Ctrl Pts',(-48.706329375,48.2291666734946,-13.0508216223155));
#11480=CARTESIAN_POINT('Ctrl Pts',(-42.1809185638422,48.0208333401613,-24.3531646875));
#11481=CARTESIAN_POINT('Ctrl Pts',(-35.6555077526845,47.812500006828,-35.6555077526845));
#11482=CARTESIAN_POINT('Ctrl Pts',(-24.3531646875,47.6041666734946,-42.1809185638422));
#11483=CARTESIAN_POINT('Ctrl Pts',(-13.0508216223155,47.3958333401613,-48.706329375));
#11484=CARTESIAN_POINT('Ctrl Pts',(1.59157945007855E-14,47.187500006828,
-48.706329375));
#11485=CARTESIAN_POINT('Ctrl Pts',(13.0508216223155,46.9791666734946,-48.706329375));
#11486=CARTESIAN_POINT('Ctrl Pts',(24.3531646875,46.7708333401613,-42.1809185638422));
#11487=CARTESIAN_POINT('Ctrl Pts',(35.6555077526845,46.562500006828,-35.6555077526845));
#11488=CARTESIAN_POINT('Ctrl Pts',(42.1809185638422,46.3541666734946,-24.3531646875));
#11489=CARTESIAN_POINT('Ctrl Pts',(48.706329375,46.1458333401613,-13.0508216223155));
#11490=CARTESIAN_POINT('Ctrl Pts',(48.706329375,45.937500006828,1.293339198242E-14));
#11491=CARTESIAN_POINT('Ctrl Pts',(48.706329375,45.7291666734946,13.0508216223155));
#11492=CARTESIAN_POINT('Ctrl Pts',(42.1809185638422,45.5208333401613,24.3531646875));
#11493=CARTESIAN_POINT('Ctrl Pts',(35.6555077526845,45.312500006828,35.6555077526845));
#11494=CARTESIAN_POINT('Ctrl Pts',(24.3531646875,45.1041666734946,42.1809185638422));
#11495=CARTESIAN_POINT('Ctrl Pts',(13.0508216223155,44.8958333401613,48.706329375));
#11496=CARTESIAN_POINT('Ctrl Pts',(-9.95098946405443E-15,44.687500006828,
48.706329375));
#11497=CARTESIAN_POINT('Ctrl Pts',(-13.0508216223155,44.4791666734946,48.706329375));
#11498=CARTESIAN_POINT('Ctrl Pts',(-24.3531646875,44.2708333401613,42.1809185638423));
#11499=CARTESIAN_POINT('Ctrl Pts',(-35.6555077526845,44.062500006828,35.6555077526845));
#11500=CARTESIAN_POINT('Ctrl Pts',(-42.1809185638422,43.8541666734946,24.3531646875));
#11501=CARTESIAN_POINT('Ctrl Pts',(-48.706329375,43.6458333401613,13.0508216223155));
#11502=CARTESIAN_POINT('Ctrl Pts',(-48.706329375,43.437500006828,-1.8898197019151E-14));
#11503=CARTESIAN_POINT('Ctrl Pts',(-48.706329375,43.2291666734946,-13.0508216223155));
#11504=CARTESIAN_POINT('Ctrl Pts',(-42.1809185638422,43.0208333401613,-24.3531646875));
#11505=CARTESIAN_POINT('Ctrl Pts',(-35.6555077526845,42.812500006828,-35.6555077526845));
#11506=CARTESIAN_POINT('Ctrl Pts',(-24.3531646875,42.6041666734946,-42.1809185638422));
#11507=CARTESIAN_POINT('Ctrl Pts',(-13.0508216223155,42.3958333401613,-48.706329375));
#11508=CARTESIAN_POINT('Ctrl Pts',(1.59157945007855E-14,42.187500006828,
-48.706329375));
#11509=CARTESIAN_POINT('Ctrl Pts',(13.0508216223155,41.9791666734946,-48.706329375));
#11510=CARTESIAN_POINT('Ctrl Pts',(24.3531646875,41.7708333401613,-42.1809185638422));
#11511=CARTESIAN_POINT('Ctrl Pts',(35.6555077526845,41.562500006828,-35.6555077526845));
#11512=CARTESIAN_POINT('Ctrl Pts',(42.1809185638422,41.3541666734946,-24.3531646875));
#11513=CARTESIAN_POINT('Ctrl Pts',(48.706329375,41.1458333401613,-13.0508216223155));
#11514=CARTESIAN_POINT('Ctrl Pts',(48.706329375,40.937500006828,1.293339198242E-14));
#11515=CARTESIAN_POINT('Ctrl Pts',(48.706329375,40.7291666734946,13.0508216223155));
#11516=CARTESIAN_POINT('Ctrl Pts',(42.1809185638422,40.5208333401613,24.3531646875));
#11517=CARTESIAN_POINT('Ctrl Pts',(35.6555077526845,40.312500006828,35.6555077526845));
#11518=CARTESIAN_POINT('Ctrl Pts',(24.3531646875,40.1041666734946,42.1809185638422));
#11519=CARTESIAN_POINT('Ctrl Pts',(13.0508216223155,39.8958333401613,48.706329375));
#11520=CARTESIAN_POINT('Ctrl Pts',(-9.95098946405443E-15,39.687500006828,
48.706329375));
#11521=CARTESIAN_POINT('Ctrl Pts',(-13.0508216223155,39.4791666734946,48.706329375));
#11522=CARTESIAN_POINT('Ctrl Pts',(-24.3531646875,39.2708333401613,42.1809185638423));
#11523=CARTESIAN_POINT('Ctrl Pts',(-35.6555077526845,39.062500006828,35.6555077526845));
#11524=CARTESIAN_POINT('Ctrl Pts',(-42.1809185638422,38.8541666734946,24.3531646875));
#11525=CARTESIAN_POINT('Ctrl Pts',(-48.706329375,38.6458333401613,13.0508216223155));
#11526=CARTESIAN_POINT('Ctrl Pts',(-48.706329375,38.437500006828,-1.8898197019151E-14));
#11527=CARTESIAN_POINT('Ctrl Pts',(-48.706329375,38.2291666734946,-13.0508216223155));
#11528=CARTESIAN_POINT('Ctrl Pts',(-42.1809185638422,38.0208333401613,-24.3531646875));
#11529=CARTESIAN_POINT('Ctrl Pts',(-35.6555077526845,37.812500006828,-35.6555077526845));
#11530=CARTESIAN_POINT('Ctrl Pts',(-24.3531646875,37.6041666734946,-42.1809185638422));
#11531=CARTESIAN_POINT('Ctrl Pts',(-13.0508216223155,37.3958333401613,-48.706329375));
#11532=CARTESIAN_POINT('Ctrl Pts',(1.59157945007855E-14,37.187500006828,
-48.706329375));
#11533=CARTESIAN_POINT('Ctrl Pts',(13.0508216223155,36.9791666734946,-48.706329375));
#11534=CARTESIAN_POINT('Ctrl Pts',(24.3531646875,36.7708333401613,-42.1809185638422));
#11535=CARTESIAN_POINT('Ctrl Pts',(35.6555077526845,36.562500006828,-35.6555077526845));
#11536=CARTESIAN_POINT('Ctrl Pts',(42.1809185638422,36.3541666734946,-24.3531646875));
#11537=CARTESIAN_POINT('Ctrl Pts',(48.706329375,36.1458333401613,-13.0508216223155));
#11538=CARTESIAN_POINT('Ctrl Pts',(48.706329375,35.937500006828,1.293339198242E-14));
#11539=CARTESIAN_POINT('Ctrl Pts',(48.706329375,35.7291666734946,13.0508216223155));
#11540=CARTESIAN_POINT('Ctrl Pts',(42.1809185638422,35.5208333401613,24.3531646875));
#11541=CARTESIAN_POINT('Ctrl Pts',(35.6555077526845,35.312500006828,35.6555077526845));
#11542=CARTESIAN_POINT('Ctrl Pts',(24.3531646875,35.1041666734946,42.1809185638422));
#11543=CARTESIAN_POINT('Ctrl Pts',(13.0508216223155,34.8958333401613,48.706329375));
#11544=CARTESIAN_POINT('Ctrl Pts',(-9.95098946405443E-15,34.687500006828,
48.706329375));
#11545=CARTESIAN_POINT('Ctrl Pts',(-13.0508216223155,34.4791666734946,48.706329375));
#11546=CARTESIAN_POINT('Ctrl Pts',(-24.3531646875,34.2708333401613,42.1809185638423));
#11547=CARTESIAN_POINT('Ctrl Pts',(-35.6555077526845,34.062500006828,35.6555077526845));
#11548=CARTESIAN_POINT('Ctrl Pts',(-42.1809185638422,33.8541666734946,24.3531646875));
#11549=CARTESIAN_POINT('Ctrl Pts',(-48.706329375,33.6458333401613,13.0508216223155));
#11550=CARTESIAN_POINT('Ctrl Pts',(-48.706329375,33.437500006828,-1.8898197019151E-14));
#11551=CARTESIAN_POINT('Ctrl Pts',(-48.706329375,33.2291666734946,-13.0508216223155));
#11552=CARTESIAN_POINT('Ctrl Pts',(-42.1809185638422,33.0208333401613,-24.3531646875));
#11553=CARTESIAN_POINT('Ctrl Pts',(-35.6555077526845,32.812500006828,-35.6555077526845));
#11554=CARTESIAN_POINT('Ctrl Pts',(-24.3531646875,32.6041666734946,-42.1809185638422));
#11555=CARTESIAN_POINT('Ctrl Pts',(-13.0508216223155,32.3958333401613,-48.706329375));
#11556=CARTESIAN_POINT('Ctrl Pts',(1.59157945007855E-14,32.187500006828,
-48.706329375));
#11557=CARTESIAN_POINT('Ctrl Pts',(13.0508216223155,31.9791666734946,-48.706329375));
#11558=CARTESIAN_POINT('Ctrl Pts',(24.3531646875,31.7708333401613,-42.1809185638422));
#11559=CARTESIAN_POINT('Ctrl Pts',(35.6555077526845,31.562500006828,-35.6555077526845));
#11560=CARTESIAN_POINT('Ctrl Pts',(42.1809185638422,31.3541666734946,-24.3531646875));
#11561=CARTESIAN_POINT('Ctrl Pts',(48.706329375,31.1458333401613,-13.0508216223155));
#11562=CARTESIAN_POINT('Ctrl Pts',(48.706329375,30.937500006828,1.293339198242E-14));
#11563=CARTESIAN_POINT('Ctrl Pts',(48.706329375,30.7291666734946,13.0508216223155));
#11564=CARTESIAN_POINT('Ctrl Pts',(42.1809185638422,30.5208333401613,24.3531646875));
#11565=CARTESIAN_POINT('Ctrl Pts',(35.6555077526845,30.312500006828,35.6555077526845));
#11566=CARTESIAN_POINT('Ctrl Pts',(24.3531646875,30.1041666734946,42.1809185638422));
#11567=CARTESIAN_POINT('Ctrl Pts',(13.0508216223155,29.8958333401613,48.706329375));
#11568=CARTESIAN_POINT('Ctrl Pts',(-9.95098946405443E-15,29.687500006828,
48.706329375));
#11569=CARTESIAN_POINT('Ctrl Pts',(-13.0508216223155,29.4791666734946,48.706329375));
#11570=CARTESIAN_POINT('Ctrl Pts',(-24.3531646875,29.2708333401613,42.1809185638423));
#11571=CARTESIAN_POINT('Ctrl Pts',(-35.6555077526845,29.062500006828,35.6555077526845));
#11572=CARTESIAN_POINT('Ctrl Pts',(-42.1809185638422,28.8541666734946,24.3531646875));
#11573=CARTESIAN_POINT('Ctrl Pts',(-48.706329375,28.6458333401613,13.0508216223155));
#11574=CARTESIAN_POINT('Ctrl Pts',(-48.706329375,28.437500006828,-1.8898197019151E-14));
#11575=CARTESIAN_POINT('Ctrl Pts',(-46.,60.,0.));
#11576=CARTESIAN_POINT('Ctrl Pts',(-46.,59.7916666666667,-12.3256628518316));
#11577=CARTESIAN_POINT('Ctrl Pts',(-39.8371685740842,59.5833333333333,-23.));
#11578=CARTESIAN_POINT('Ctrl Pts',(-33.6743371481684,59.375,-33.6743371481684));
#11579=CARTESIAN_POINT('Ctrl Pts',(-23.,59.1666666666667,-39.8371685740842));
#11580=CARTESIAN_POINT('Ctrl Pts',(-12.3256628518317,58.9583333333333,-46.));
#11581=CARTESIAN_POINT('Ctrl Pts',(-2.81668763803891E-15,58.75,-46.));
#11582=CARTESIAN_POINT('Ctrl Pts',(12.3256628518316,58.5416666666667,-46.));
#11583=CARTESIAN_POINT('Ctrl Pts',(23.,58.3333333333333,-39.8371685740842));
#11584=CARTESIAN_POINT('Ctrl Pts',(33.6743371481683,58.125,-33.6743371481684));
#11585=CARTESIAN_POINT('Ctrl Pts',(39.8371685740842,57.9166666666667,-23.));
#11586=CARTESIAN_POINT('Ctrl Pts',(46.,57.7083333333333,-12.3256628518317));
#11587=CARTESIAN_POINT('Ctrl Pts',(46.,57.5,-5.63337527607782E-15));
#11588=CARTESIAN_POINT('Ctrl Pts',(46.,57.2916666666667,12.3256628518316));
#11589=CARTESIAN_POINT('Ctrl Pts',(39.8371685740842,57.0833333333333,23.));
#11590=CARTESIAN_POINT('Ctrl Pts',(33.6743371481684,56.875,33.6743371481683));
#11591=CARTESIAN_POINT('Ctrl Pts',(23.,56.6666666666667,39.8371685740842));
#11592=CARTESIAN_POINT('Ctrl Pts',(12.3256628518317,56.4583333333333,46.));
#11593=CARTESIAN_POINT('Ctrl Pts',(8.45006291411674E-15,56.25,46.));
#11594=CARTESIAN_POINT('Ctrl Pts',(-12.3256628518316,56.0416666666667,46.));
#11595=CARTESIAN_POINT('Ctrl Pts',(-23.,55.8333333333333,39.8371685740842));
#11596=CARTESIAN_POINT('Ctrl Pts',(-33.6743371481683,55.625,33.6743371481684));
#11597=CARTESIAN_POINT('Ctrl Pts',(-39.8371685740842,55.4166666666667,23.));
#11598=CARTESIAN_POINT('Ctrl Pts',(-46.,55.2083333333333,12.3256628518317));
#11599=CARTESIAN_POINT('Ctrl Pts',(-46.,55.,0.));
#11600=CARTESIAN_POINT('Ctrl Pts',(-46.,54.7916666666667,-12.3256628518316));
#11601=CARTESIAN_POINT('Ctrl Pts',(-39.8371685740842,54.5833333333333,-23.));
#11602=CARTESIAN_POINT('Ctrl Pts',(-33.6743371481684,54.375,-33.6743371481684));
#11603=CARTESIAN_POINT('Ctrl Pts',(-23.,54.1666666666667,-39.8371685740842));
#11604=CARTESIAN_POINT('Ctrl Pts',(-12.3256628518317,53.9583333333333,-46.));
#11605=CARTESIAN_POINT('Ctrl Pts',(-2.81668763803891E-15,53.75,-46.));
#11606=CARTESIAN_POINT('Ctrl Pts',(12.3256628518316,53.5416666666667,-46.));
#11607=CARTESIAN_POINT('Ctrl Pts',(23.,53.3333333333333,-39.8371685740842));
#11608=CARTESIAN_POINT('Ctrl Pts',(33.6743371481683,53.125,-33.6743371481684));
#11609=CARTESIAN_POINT('Ctrl Pts',(39.8371685740842,52.9166666666667,-23.));
#11610=CARTESIAN_POINT('Ctrl Pts',(46.,52.7083333333333,-12.3256628518317));
#11611=CARTESIAN_POINT('Ctrl Pts',(46.,52.5,-5.63337527607782E-15));
#11612=CARTESIAN_POINT('Ctrl Pts',(46.,52.2916666666667,12.3256628518316));
#11613=CARTESIAN_POINT('Ctrl Pts',(39.8371685740842,52.0833333333333,23.));
#11614=CARTESIAN_POINT('Ctrl Pts',(33.6743371481684,51.875,33.6743371481683));
#11615=CARTESIAN_POINT('Ctrl Pts',(23.,51.6666666666667,39.8371685740842));
#11616=CARTESIAN_POINT('Ctrl Pts',(12.3256628518317,51.4583333333333,46.));
#11617=CARTESIAN_POINT('Ctrl Pts',(8.45006291411674E-15,51.25,46.));
#11618=CARTESIAN_POINT('Ctrl Pts',(-12.3256628518316,51.0416666666667,46.));
#11619=CARTESIAN_POINT('Ctrl Pts',(-23.,50.8333333333333,39.8371685740842));
#11620=CARTESIAN_POINT('Ctrl Pts',(-33.6743371481683,50.625,33.6743371481684));
#11621=CARTESIAN_POINT('Ctrl Pts',(-39.8371685740842,50.4166666666667,23.));
#11622=CARTESIAN_POINT('Ctrl Pts',(-46.,50.2083333333333,12.3256628518317));
#11623=CARTESIAN_POINT('Ctrl Pts',(-46.,50.,0.));
#11624=CARTESIAN_POINT('Ctrl Pts',(-46.,49.7916666666667,-12.3256628518316));
#11625=CARTESIAN_POINT('Ctrl Pts',(-39.8371685740842,49.5833333333333,-23.));
#11626=CARTESIAN_POINT('Ctrl Pts',(-33.6743371481684,49.375,-33.6743371481684));
#11627=CARTESIAN_POINT('Ctrl Pts',(-23.,49.1666666666667,-39.8371685740842));
#11628=CARTESIAN_POINT('Ctrl Pts',(-12.3256628518317,48.9583333333333,-46.));
#11629=CARTESIAN_POINT('Ctrl Pts',(-2.81668763803891E-15,48.75,-46.));
#11630=CARTESIAN_POINT('Ctrl Pts',(12.3256628518316,48.5416666666667,-46.));
#11631=CARTESIAN_POINT('Ctrl Pts',(23.,48.3333333333333,-39.8371685740842));
#11632=CARTESIAN_POINT('Ctrl Pts',(33.6743371481683,48.125,-33.6743371481684));
#11633=CARTESIAN_POINT('Ctrl Pts',(39.8371685740842,47.9166666666667,-23.));
#11634=CARTESIAN_POINT('Ctrl Pts',(46.,47.7083333333333,-12.3256628518317));
#11635=CARTESIAN_POINT('Ctrl Pts',(46.,47.5,-5.63337527607782E-15));
#11636=CARTESIAN_POINT('Ctrl Pts',(46.,47.2916666666667,12.3256628518316));
#11637=CARTESIAN_POINT('Ctrl Pts',(39.8371685740842,47.0833333333333,23.));
#11638=CARTESIAN_POINT('Ctrl Pts',(33.6743371481684,46.875,33.6743371481683));
#11639=CARTESIAN_POINT('Ctrl Pts',(23.,46.6666666666667,39.8371685740842));
#11640=CARTESIAN_POINT('Ctrl Pts',(12.3256628518317,46.4583333333333,46.));
#11641=CARTESIAN_POINT('Ctrl Pts',(8.45006291411674E-15,46.25,46.));
#11642=CARTESIAN_POINT('Ctrl Pts',(-12.3256628518316,46.0416666666667,46.));
#11643=CARTESIAN_POINT('Ctrl Pts',(-23.,45.8333333333333,39.8371685740842));
#11644=CARTESIAN_POINT('Ctrl Pts',(-33.6743371481683,45.625,33.6743371481684));
#11645=CARTESIAN_POINT('Ctrl Pts',(-39.8371685740842,45.4166666666667,23.));
#11646=CARTESIAN_POINT('Ctrl Pts',(-46.,45.2083333333333,12.3256628518317));
#11647=CARTESIAN_POINT('Ctrl Pts',(-46.,45.,0.));
#11648=CARTESIAN_POINT('Ctrl Pts',(-46.,44.7916666666667,-12.3256628518316));
#11649=CARTESIAN_POINT('Ctrl Pts',(-39.8371685740842,44.5833333333333,-23.));
#11650=CARTESIAN_POINT('Ctrl Pts',(-33.6743371481684,44.375,-33.6743371481684));
#11651=CARTESIAN_POINT('Ctrl Pts',(-23.,44.1666666666667,-39.8371685740842));
#11652=CARTESIAN_POINT('Ctrl Pts',(-12.3256628518317,43.9583333333333,-46.));
#11653=CARTESIAN_POINT('Ctrl Pts',(-2.81668763803891E-15,43.75,-46.));
#11654=CARTESIAN_POINT('Ctrl Pts',(12.3256628518316,43.5416666666667,-46.));
#11655=CARTESIAN_POINT('Ctrl Pts',(23.,43.3333333333333,-39.8371685740842));
#11656=CARTESIAN_POINT('Ctrl Pts',(33.6743371481683,43.125,-33.6743371481684));
#11657=CARTESIAN_POINT('Ctrl Pts',(39.8371685740842,42.9166666666667,-23.));
#11658=CARTESIAN_POINT('Ctrl Pts',(46.,42.7083333333333,-12.3256628518317));
#11659=CARTESIAN_POINT('Ctrl Pts',(46.,42.5,-5.63337527607782E-15));
#11660=CARTESIAN_POINT('Ctrl Pts',(46.,42.2916666666667,12.3256628518316));
#11661=CARTESIAN_POINT('Ctrl Pts',(39.8371685740842,42.0833333333333,23.));
#11662=CARTESIAN_POINT('Ctrl Pts',(33.6743371481684,41.875,33.6743371481683));
#11663=CARTESIAN_POINT('Ctrl Pts',(23.,41.6666666666667,39.8371685740842));
#11664=CARTESIAN_POINT('Ctrl Pts',(12.3256628518317,41.4583333333333,46.));
#11665=CARTESIAN_POINT('Ctrl Pts',(8.45006291411674E-15,41.25,46.));
#11666=CARTESIAN_POINT('Ctrl Pts',(-12.3256628518316,41.0416666666667,46.));
#11667=CARTESIAN_POINT('Ctrl Pts',(-23.,40.8333333333333,39.8371685740842));
#11668=CARTESIAN_POINT('Ctrl Pts',(-33.6743371481683,40.625,33.6743371481684));
#11669=CARTESIAN_POINT('Ctrl Pts',(-39.8371685740842,40.4166666666667,23.));
#11670=CARTESIAN_POINT('Ctrl Pts',(-46.,40.2083333333333,12.3256628518317));
#11671=CARTESIAN_POINT('Ctrl Pts',(-46.,40.,0.));
#11672=CARTESIAN_POINT('Ctrl Pts',(-46.,39.7916666666667,-12.3256628518316));
#11673=CARTESIAN_POINT('Ctrl Pts',(-39.8371685740842,39.5833333333333,-23.));
#11674=CARTESIAN_POINT('Ctrl Pts',(-33.6743371481684,39.375,-33.6743371481684));
#11675=CARTESIAN_POINT('Ctrl Pts',(-23.,39.1666666666667,-39.8371685740842));
#11676=CARTESIAN_POINT('Ctrl Pts',(-12.3256628518317,38.9583333333333,-46.));
#11677=CARTESIAN_POINT('Ctrl Pts',(-2.81668763803891E-15,38.75,-46.));
#11678=CARTESIAN_POINT('Ctrl Pts',(12.3256628518316,38.5416666666667,-46.));
#11679=CARTESIAN_POINT('Ctrl Pts',(23.,38.3333333333333,-39.8371685740842));
#11680=CARTESIAN_POINT('Ctrl Pts',(33.6743371481683,38.125,-33.6743371481684));
#11681=CARTESIAN_POINT('Ctrl Pts',(39.8371685740842,37.9166666666667,-23.));
#11682=CARTESIAN_POINT('Ctrl Pts',(46.,37.7083333333333,-12.3256628518317));
#11683=CARTESIAN_POINT('Ctrl Pts',(46.,37.5,-5.63337527607782E-15));
#11684=CARTESIAN_POINT('Ctrl Pts',(46.,37.2916666666667,12.3256628518316));
#11685=CARTESIAN_POINT('Ctrl Pts',(39.8371685740842,37.0833333333333,23.));
#11686=CARTESIAN_POINT('Ctrl Pts',(33.6743371481684,36.875,33.6743371481683));
#11687=CARTESIAN_POINT('Ctrl Pts',(23.,36.6666666666667,39.8371685740842));
#11688=CARTESIAN_POINT('Ctrl Pts',(12.3256628518317,36.4583333333333,46.));
#11689=CARTESIAN_POINT('Ctrl Pts',(8.45006291411674E-15,36.25,46.));
#11690=CARTESIAN_POINT('Ctrl Pts',(-12.3256628518316,36.0416666666667,46.));
#11691=CARTESIAN_POINT('Ctrl Pts',(-23.,35.8333333333333,39.8371685740842));
#11692=CARTESIAN_POINT('Ctrl Pts',(-33.6743371481683,35.625,33.6743371481684));
#11693=CARTESIAN_POINT('Ctrl Pts',(-39.8371685740842,35.4166666666667,23.));
#11694=CARTESIAN_POINT('Ctrl Pts',(-46.,35.2083333333333,12.3256628518317));
#11695=CARTESIAN_POINT('Ctrl Pts',(-46.,35.,0.));
#11696=CARTESIAN_POINT('Ctrl Pts',(-46.,34.7916666666667,-12.3256628518316));
#11697=CARTESIAN_POINT('Ctrl Pts',(-39.8371685740842,34.5833333333333,-23.));
#11698=CARTESIAN_POINT('Ctrl Pts',(-33.6743371481684,34.375,-33.6743371481684));
#11699=CARTESIAN_POINT('Ctrl Pts',(-23.,34.1666666666667,-39.8371685740842));
#11700=CARTESIAN_POINT('Ctrl Pts',(-12.3256628518317,33.9583333333333,-46.));
#11701=CARTESIAN_POINT('Ctrl Pts',(-2.81668763803891E-15,33.75,-46.));
#11702=CARTESIAN_POINT('Ctrl Pts',(12.3256628518316,33.5416666666667,-46.));
#11703=CARTESIAN_POINT('Ctrl Pts',(23.,33.3333333333333,-39.8371685740842));
#11704=CARTESIAN_POINT('Ctrl Pts',(33.6743371481683,33.125,-33.6743371481684));
#11705=CARTESIAN_POINT('Ctrl Pts',(39.8371685740842,32.9166666666667,-23.));
#11706=CARTESIAN_POINT('Ctrl Pts',(46.,32.7083333333333,-12.3256628518317));
#11707=CARTESIAN_POINT('Ctrl Pts',(46.,32.5,-5.63337527607782E-15));
#11708=CARTESIAN_POINT('Ctrl Pts',(46.,32.2916666666667,12.3256628518316));
#11709=CARTESIAN_POINT('Ctrl Pts',(39.8371685740842,32.0833333333333,23.));
#11710=CARTESIAN_POINT('Ctrl Pts',(33.6743371481684,31.875,33.6743371481683));
#11711=CARTESIAN_POINT('Ctrl Pts',(23.,31.6666666666667,39.8371685740842));
#11712=CARTESIAN_POINT('Ctrl Pts',(12.3256628518317,31.4583333333333,46.));
#11713=CARTESIAN_POINT('Ctrl Pts',(8.45006291411674E-15,31.25,46.));
#11714=CARTESIAN_POINT('Ctrl Pts',(-12.3256628518316,31.0416666666667,46.));
#11715=CARTESIAN_POINT('Ctrl Pts',(-23.,30.8333333333333,39.8371685740842));
#11716=CARTESIAN_POINT('Ctrl Pts',(-33.6743371481683,30.625,33.6743371481684));
#11717=CARTESIAN_POINT('Ctrl Pts',(-39.8371685740842,30.4166666666667,23.));
#11718=CARTESIAN_POINT('Ctrl Pts',(-46.,30.2083333333333,12.3256628518317));
#11719=CARTESIAN_POINT('Ctrl Pts',(-46.,30.,0.));
#11720=CARTESIAN_POINT('',(46.6217457715553,57.,3.60701400320327));
#11721=CARTESIAN_POINT('Ctrl Pts',(48.5725845633798,55.8793483229262,3.60701400320328));
#11722=CARTESIAN_POINT('Ctrl Pts',(48.3407853679392,56.0125314497137,3.60701400320328));
#11723=CARTESIAN_POINT('Ctrl Pts',(48.1089821836664,56.1457076343818,3.60701400320327));
#11724=CARTESIAN_POINT('Ctrl Pts',(47.6453674864979,56.4120455056142,3.60701400320327));
#11725=CARTESIAN_POINT('Ctrl Pts',(47.4135559734254,56.5452071923974,3.60701400320327));
#11726=CARTESIAN_POINT('Ctrl Pts',(47.1817401099609,56.6783613050641,3.60701400320327));
#11727=CARTESIAN_POINT('Ctrl Pts',(46.995078185609,56.7855791741705,3.60701400320327));
#11728=CARTESIAN_POINT('Ctrl Pts',(46.8084134402483,56.8927921321767,3.60701400320327));
#11729=CARTESIAN_POINT('Ctrl Pts',(46.6217457715553,57.,3.60701400320327));
#11730=CARTESIAN_POINT('',(37.183468849883,57.,27.0811677054329));
#11731=CARTESIAN_POINT('Ctrl Pts',(46.6217457715554,57.,3.60701400320327));
#11732=CARTESIAN_POINT('Ctrl Pts',(46.1677264415782,57.,7.85340573112802));
#11733=CARTESIAN_POINT('Ctrl Pts',(45.1307231920318,57.,12.0169900453439));
#11734=CARTESIAN_POINT('Ctrl Pts',(41.9496451502407,57.,19.9424594354284));
#11735=CARTESIAN_POINT('Ctrl Pts',(39.8111418078332,57.,23.691305179069));
#11736=CARTESIAN_POINT('Ctrl Pts',(37.183468849883,57.,27.0811677054329));
#11737=CARTESIAN_POINT('',(3.61292728433799,56.311710737147,45.8578974271399));
#11738=CARTESIAN_POINT('Ctrl Pts',(37.183468849883,57.,27.0811677054329));
#11739=CARTESIAN_POINT('Ctrl Pts',(31.4435637667069,56.8314615162496,34.9622747604562));
#11740=CARTESIAN_POINT('Ctrl Pts',(23.,56.6666666666667,39.8371685740842));
#11741=CARTESIAN_POINT('Ctrl Pts',(13.9875081498766,56.4907679253478,45.0405331698223));
#11742=CARTESIAN_POINT('Ctrl Pts',(3.61292728433799,56.311710737147,45.8578974271399));
#11743=CARTESIAN_POINT('Ctrl Pts',(3.61292728433799,56.311710737147,45.8578974271399));
#11744=CARTESIAN_POINT('Ctrl Pts',(3.612927284338,56.178117727701,46.089460636719));
#11745=CARTESIAN_POINT('Ctrl Pts',(3.61292728433797,55.9109294856547,46.5525857733052));
#11746=CARTESIAN_POINT('Ctrl Pts',(3.61292728433799,55.6437369897944,47.0157084557285));
#11747=CARTESIAN_POINT('Ctrl Pts',(3.61292728433799,55.2553460757965,47.6888965792834));
#11748=CARTESIAN_POINT('Ctrl Pts',(3.612927284338,55.0005487265709,48.1305218136162));
#11749=CARTESIAN_POINT('Ctrl Pts',(3.612927284338,54.7457479656467,48.5721450795008));
#11750=CARTESIAN_POINT('Ctrl Pts',(-48.706329375,58.437500006828,-1.8898197019151E-14));
#11751=CARTESIAN_POINT('Ctrl Pts',(-48.706329375,58.2291666734946,-13.0508216223155));
#11752=CARTESIAN_POINT('Ctrl Pts',(-42.1809185638422,58.0208333401613,-24.3531646875));
#11753=CARTESIAN_POINT('Ctrl Pts',(-35.6555077526845,57.812500006828,-35.6555077526845));
#11754=CARTESIAN_POINT('Ctrl Pts',(-24.3531646875,57.6041666734946,-42.1809185638422));
#11755=CARTESIAN_POINT('Ctrl Pts',(-13.0508216223155,57.3958333401613,-48.706329375));
#11756=CARTESIAN_POINT('Ctrl Pts',(1.59157945007855E-14,57.187500006828,
-48.706329375));
#11757=CARTESIAN_POINT('Ctrl Pts',(13.0508216223155,56.9791666734946,-48.706329375));
#11758=CARTESIAN_POINT('Ctrl Pts',(24.3531646875,56.7708333401613,-42.1809185638422));
#11759=CARTESIAN_POINT('Ctrl Pts',(35.6555077526845,56.562500006828,-35.6555077526845));
#11760=CARTESIAN_POINT('Ctrl Pts',(42.1809185638422,56.3541666734946,-24.3531646875));
#11761=CARTESIAN_POINT('Ctrl Pts',(48.706329375,56.1458333401613,-13.0508216223155));
#11762=CARTESIAN_POINT('Ctrl Pts',(48.706329375,55.937500006828,1.293339198242E-14));
#11763=CARTESIAN_POINT('Ctrl Pts',(48.706329375,55.7291666734946,13.0508216223155));
#11764=CARTESIAN_POINT('Ctrl Pts',(42.1809185638422,55.5208333401613,24.3531646875));
#11765=CARTESIAN_POINT('Ctrl Pts',(35.6555077526845,55.312500006828,35.6555077526845));
#11766=CARTESIAN_POINT('Ctrl Pts',(24.3531646875,55.1041666734946,42.1809185638422));
#11767=CARTESIAN_POINT('Ctrl Pts',(13.0508216223155,54.8958333401613,48.706329375));
#11768=CARTESIAN_POINT('Ctrl Pts',(-9.95098946405443E-15,54.687500006828,
48.706329375));
#11769=CARTESIAN_POINT('Ctrl Pts',(-13.0508216223155,54.4791666734946,48.706329375));
#11770=CARTESIAN_POINT('Ctrl Pts',(-24.3531646875,54.2708333401613,42.1809185638423));
#11771=CARTESIAN_POINT('Ctrl Pts',(-35.6555077526845,54.062500006828,35.6555077526845));
#11772=CARTESIAN_POINT('Ctrl Pts',(-42.1809185638422,53.8541666734946,24.3531646875));
#11773=CARTESIAN_POINT('Ctrl Pts',(-48.706329375,53.6458333401613,13.0508216223155));
#11774=CARTESIAN_POINT('Ctrl Pts',(-48.706329375,53.437500006828,-1.8898197019151E-14));
#11775=CARTESIAN_POINT('Ctrl Pts',(-48.706329375,53.2291666734946,-13.0508216223155));
#11776=CARTESIAN_POINT('Ctrl Pts',(-42.1809185638422,53.0208333401613,-24.3531646875));
#11777=CARTESIAN_POINT('Ctrl Pts',(-35.6555077526845,52.812500006828,-35.6555077526845));
#11778=CARTESIAN_POINT('Ctrl Pts',(-24.3531646875,52.6041666734946,-42.1809185638422));
#11779=CARTESIAN_POINT('Ctrl Pts',(-13.0508216223155,52.3958333401613,-48.706329375));
#11780=CARTESIAN_POINT('Ctrl Pts',(1.59157945007855E-14,52.187500006828,
-48.706329375));
#11781=CARTESIAN_POINT('Ctrl Pts',(13.0508216223155,51.9791666734946,-48.706329375));
#11782=CARTESIAN_POINT('Ctrl Pts',(24.3531646875,51.7708333401613,-42.1809185638422));
#11783=CARTESIAN_POINT('Ctrl Pts',(35.6555077526845,51.562500006828,-35.6555077526845));
#11784=CARTESIAN_POINT('Ctrl Pts',(42.1809185638422,51.3541666734946,-24.3531646875));
#11785=CARTESIAN_POINT('Ctrl Pts',(48.706329375,51.1458333401613,-13.0508216223155));
#11786=CARTESIAN_POINT('Ctrl Pts',(48.706329375,50.937500006828,1.293339198242E-14));
#11787=CARTESIAN_POINT('Ctrl Pts',(48.706329375,50.7291666734946,13.0508216223155));
#11788=CARTESIAN_POINT('Ctrl Pts',(42.1809185638422,50.5208333401613,24.3531646875));
#11789=CARTESIAN_POINT('Ctrl Pts',(35.6555077526845,50.312500006828,35.6555077526845));
#11790=CARTESIAN_POINT('Ctrl Pts',(24.3531646875,50.1041666734946,42.1809185638422));
#11791=CARTESIAN_POINT('Ctrl Pts',(13.0508216223155,49.8958333401613,48.706329375));
#11792=CARTESIAN_POINT('Ctrl Pts',(-9.95098946405443E-15,49.687500006828,
48.706329375));
#11793=CARTESIAN_POINT('Ctrl Pts',(-13.0508216223155,49.4791666734946,48.706329375));
#11794=CARTESIAN_POINT('Ctrl Pts',(-24.3531646875,49.2708333401613,42.1809185638423));
#11795=CARTESIAN_POINT('Ctrl Pts',(-35.6555077526845,49.062500006828,35.6555077526845));
#11796=CARTESIAN_POINT('Ctrl Pts',(-42.1809185638422,48.8541666734946,24.3531646875));
#11797=CARTESIAN_POINT('Ctrl Pts',(-48.706329375,48.6458333401613,13.0508216223155));
#11798=CARTESIAN_POINT('Ctrl Pts',(-48.706329375,48.437500006828,-1.8898197019151E-14));
#11799=CARTESIAN_POINT('Ctrl Pts',(-48.706329375,48.2291666734946,-13.0508216223155));
#11800=CARTESIAN_POINT('Ctrl Pts',(-42.1809185638422,48.0208333401613,-24.3531646875));
#11801=CARTESIAN_POINT('Ctrl Pts',(-35.6555077526845,47.812500006828,-35.6555077526845));
#11802=CARTESIAN_POINT('Ctrl Pts',(-24.3531646875,47.6041666734946,-42.1809185638422));
#11803=CARTESIAN_POINT('Ctrl Pts',(-13.0508216223155,47.3958333401613,-48.706329375));
#11804=CARTESIAN_POINT('Ctrl Pts',(1.59157945007855E-14,47.187500006828,
-48.706329375));
#11805=CARTESIAN_POINT('Ctrl Pts',(13.0508216223155,46.9791666734946,-48.706329375));
#11806=CARTESIAN_POINT('Ctrl Pts',(24.3531646875,46.7708333401613,-42.1809185638422));
#11807=CARTESIAN_POINT('Ctrl Pts',(35.6555077526845,46.562500006828,-35.6555077526845));
#11808=CARTESIAN_POINT('Ctrl Pts',(42.1809185638422,46.3541666734946,-24.3531646875));
#11809=CARTESIAN_POINT('Ctrl Pts',(48.706329375,46.1458333401613,-13.0508216223155));
#11810=CARTESIAN_POINT('Ctrl Pts',(48.706329375,45.937500006828,1.293339198242E-14));
#11811=CARTESIAN_POINT('Ctrl Pts',(48.706329375,45.7291666734946,13.0508216223155));
#11812=CARTESIAN_POINT('Ctrl Pts',(42.1809185638422,45.5208333401613,24.3531646875));
#11813=CARTESIAN_POINT('Ctrl Pts',(35.6555077526845,45.312500006828,35.6555077526845));
#11814=CARTESIAN_POINT('Ctrl Pts',(24.3531646875,45.1041666734946,42.1809185638422));
#11815=CARTESIAN_POINT('Ctrl Pts',(13.0508216223155,44.8958333401613,48.706329375));
#11816=CARTESIAN_POINT('Ctrl Pts',(-9.95098946405443E-15,44.687500006828,
48.706329375));
#11817=CARTESIAN_POINT('Ctrl Pts',(-13.0508216223155,44.4791666734946,48.706329375));
#11818=CARTESIAN_POINT('Ctrl Pts',(-24.3531646875,44.2708333401613,42.1809185638423));
#11819=CARTESIAN_POINT('Ctrl Pts',(-35.6555077526845,44.062500006828,35.6555077526845));
#11820=CARTESIAN_POINT('Ctrl Pts',(-42.1809185638422,43.8541666734946,24.3531646875));
#11821=CARTESIAN_POINT('Ctrl Pts',(-48.706329375,43.6458333401613,13.0508216223155));
#11822=CARTESIAN_POINT('Ctrl Pts',(-48.706329375,43.437500006828,-1.8898197019151E-14));
#11823=CARTESIAN_POINT('Ctrl Pts',(-48.706329375,43.2291666734946,-13.0508216223155));
#11824=CARTESIAN_POINT('Ctrl Pts',(-42.1809185638422,43.0208333401613,-24.3531646875));
#11825=CARTESIAN_POINT('Ctrl Pts',(-35.6555077526845,42.812500006828,-35.6555077526845));
#11826=CARTESIAN_POINT('Ctrl Pts',(-24.3531646875,42.6041666734946,-42.1809185638422));
#11827=CARTESIAN_POINT('Ctrl Pts',(-13.0508216223155,42.3958333401613,-48.706329375));
#11828=CARTESIAN_POINT('Ctrl Pts',(1.59157945007855E-14,42.187500006828,
-48.706329375));
#11829=CARTESIAN_POINT('Ctrl Pts',(13.0508216223155,41.9791666734946,-48.706329375));
#11830=CARTESIAN_POINT('Ctrl Pts',(24.3531646875,41.7708333401613,-42.1809185638422));
#11831=CARTESIAN_POINT('Ctrl Pts',(35.6555077526845,41.562500006828,-35.6555077526845));
#11832=CARTESIAN_POINT('Ctrl Pts',(42.1809185638422,41.3541666734946,-24.3531646875));
#11833=CARTESIAN_POINT('Ctrl Pts',(48.706329375,41.1458333401613,-13.0508216223155));
#11834=CARTESIAN_POINT('Ctrl Pts',(48.706329375,40.937500006828,1.293339198242E-14));
#11835=CARTESIAN_POINT('Ctrl Pts',(48.706329375,40.7291666734946,13.0508216223155));
#11836=CARTESIAN_POINT('Ctrl Pts',(42.1809185638422,40.5208333401613,24.3531646875));
#11837=CARTESIAN_POINT('Ctrl Pts',(35.6555077526845,40.312500006828,35.6555077526845));
#11838=CARTESIAN_POINT('Ctrl Pts',(24.3531646875,40.1041666734946,42.1809185638422));
#11839=CARTESIAN_POINT('Ctrl Pts',(13.0508216223155,39.8958333401613,48.706329375));
#11840=CARTESIAN_POINT('Ctrl Pts',(-9.95098946405443E-15,39.687500006828,
48.706329375));
#11841=CARTESIAN_POINT('Ctrl Pts',(-13.0508216223155,39.4791666734946,48.706329375));
#11842=CARTESIAN_POINT('Ctrl Pts',(-24.3531646875,39.2708333401613,42.1809185638423));
#11843=CARTESIAN_POINT('Ctrl Pts',(-35.6555077526845,39.062500006828,35.6555077526845));
#11844=CARTESIAN_POINT('Ctrl Pts',(-42.1809185638422,38.8541666734946,24.3531646875));
#11845=CARTESIAN_POINT('Ctrl Pts',(-48.706329375,38.6458333401613,13.0508216223155));
#11846=CARTESIAN_POINT('Ctrl Pts',(-48.706329375,38.437500006828,-1.8898197019151E-14));
#11847=CARTESIAN_POINT('Ctrl Pts',(-48.706329375,38.2291666734946,-13.0508216223155));
#11848=CARTESIAN_POINT('Ctrl Pts',(-42.1809185638422,38.0208333401613,-24.3531646875));
#11849=CARTESIAN_POINT('Ctrl Pts',(-35.6555077526845,37.812500006828,-35.6555077526845));
#11850=CARTESIAN_POINT('Ctrl Pts',(-24.3531646875,37.6041666734946,-42.1809185638422));
#11851=CARTESIAN_POINT('Ctrl Pts',(-13.0508216223155,37.3958333401613,-48.706329375));
#11852=CARTESIAN_POINT('Ctrl Pts',(1.59157945007855E-14,37.187500006828,
-48.706329375));
#11853=CARTESIAN_POINT('Ctrl Pts',(13.0508216223155,36.9791666734946,-48.706329375));
#11854=CARTESIAN_POINT('Ctrl Pts',(24.3531646875,36.7708333401613,-42.1809185638422));
#11855=CARTESIAN_POINT('Ctrl Pts',(35.6555077526845,36.562500006828,-35.6555077526845));
#11856=CARTESIAN_POINT('Ctrl Pts',(42.1809185638422,36.3541666734946,-24.3531646875));
#11857=CARTESIAN_POINT('Ctrl Pts',(48.706329375,36.1458333401613,-13.0508216223155));
#11858=CARTESIAN_POINT('Ctrl Pts',(48.706329375,35.937500006828,1.293339198242E-14));
#11859=CARTESIAN_POINT('Ctrl Pts',(48.706329375,35.7291666734946,13.0508216223155));
#11860=CARTESIAN_POINT('Ctrl Pts',(42.1809185638422,35.5208333401613,24.3531646875));
#11861=CARTESIAN_POINT('Ctrl Pts',(35.6555077526845,35.312500006828,35.6555077526845));
#11862=CARTESIAN_POINT('Ctrl Pts',(24.3531646875,35.1041666734946,42.1809185638422));
#11863=CARTESIAN_POINT('Ctrl Pts',(13.0508216223155,34.8958333401613,48.706329375));
#11864=CARTESIAN_POINT('Ctrl Pts',(-9.95098946405443E-15,34.687500006828,
48.706329375));
#11865=CARTESIAN_POINT('Ctrl Pts',(-13.0508216223155,34.4791666734946,48.706329375));
#11866=CARTESIAN_POINT('Ctrl Pts',(-24.3531646875,34.2708333401613,42.1809185638423));
#11867=CARTESIAN_POINT('Ctrl Pts',(-35.6555077526845,34.062500006828,35.6555077526845));
#11868=CARTESIAN_POINT('Ctrl Pts',(-42.1809185638422,33.8541666734946,24.3531646875));
#11869=CARTESIAN_POINT('Ctrl Pts',(-48.706329375,33.6458333401613,13.0508216223155));
#11870=CARTESIAN_POINT('Ctrl Pts',(-48.706329375,33.437500006828,-1.8898197019151E-14));
#11871=CARTESIAN_POINT('Ctrl Pts',(-48.706329375,33.2291666734946,-13.0508216223155));
#11872=CARTESIAN_POINT('Ctrl Pts',(-42.1809185638422,33.0208333401613,-24.3531646875));
#11873=CARTESIAN_POINT('Ctrl Pts',(-35.6555077526845,32.812500006828,-35.6555077526845));
#11874=CARTESIAN_POINT('Ctrl Pts',(-24.3531646875,32.6041666734946,-42.1809185638422));
#11875=CARTESIAN_POINT('Ctrl Pts',(-13.0508216223155,32.3958333401613,-48.706329375));
#11876=CARTESIAN_POINT('Ctrl Pts',(1.59157945007855E-14,32.187500006828,
-48.706329375));
#11877=CARTESIAN_POINT('Ctrl Pts',(13.0508216223155,31.9791666734946,-48.706329375));
#11878=CARTESIAN_POINT('Ctrl Pts',(24.3531646875,31.7708333401613,-42.1809185638422));
#11879=CARTESIAN_POINT('Ctrl Pts',(35.6555077526845,31.562500006828,-35.6555077526845));
#11880=CARTESIAN_POINT('Ctrl Pts',(42.1809185638422,31.3541666734946,-24.3531646875));
#11881=CARTESIAN_POINT('Ctrl Pts',(48.706329375,31.1458333401613,-13.0508216223155));
#11882=CARTESIAN_POINT('Ctrl Pts',(48.706329375,30.937500006828,1.293339198242E-14));
#11883=CARTESIAN_POINT('Ctrl Pts',(48.706329375,30.7291666734946,13.0508216223155));
#11884=CARTESIAN_POINT('Ctrl Pts',(42.1809185638422,30.5208333401613,24.3531646875));
#11885=CARTESIAN_POINT('Ctrl Pts',(35.6555077526845,30.312500006828,35.6555077526845));
#11886=CARTESIAN_POINT('Ctrl Pts',(24.3531646875,30.1041666734946,42.1809185638422));
#11887=CARTESIAN_POINT('Ctrl Pts',(13.0508216223155,29.8958333401613,48.706329375));
#11888=CARTESIAN_POINT('Ctrl Pts',(-9.95098946405443E-15,29.687500006828,
48.706329375));
#11889=CARTESIAN_POINT('Ctrl Pts',(-13.0508216223155,29.4791666734946,48.706329375));
#11890=CARTESIAN_POINT('Ctrl Pts',(-24.3531646875,29.2708333401613,42.1809185638423));
#11891=CARTESIAN_POINT('Ctrl Pts',(-35.6555077526845,29.062500006828,35.6555077526845));
#11892=CARTESIAN_POINT('Ctrl Pts',(-42.1809185638422,28.8541666734946,24.3531646875));
#11893=CARTESIAN_POINT('Ctrl Pts',(-48.706329375,28.6458333401613,13.0508216223155));
#11894=CARTESIAN_POINT('Ctrl Pts',(-48.706329375,28.437500006828,-1.8898197019151E-14));
#11895=CARTESIAN_POINT('Ctrl Pts',(-46.,60.,0.));
#11896=CARTESIAN_POINT('Ctrl Pts',(-46.,59.7916666666667,-12.3256628518316));
#11897=CARTESIAN_POINT('Ctrl Pts',(-39.8371685740842,59.5833333333333,-23.));
#11898=CARTESIAN_POINT('Ctrl Pts',(-33.6743371481684,59.375,-33.6743371481684));
#11899=CARTESIAN_POINT('Ctrl Pts',(-23.,59.1666666666667,-39.8371685740842));
#11900=CARTESIAN_POINT('Ctrl Pts',(-12.3256628518317,58.9583333333333,-46.));
#11901=CARTESIAN_POINT('Ctrl Pts',(-2.81668763803891E-15,58.75,-46.));
#11902=CARTESIAN_POINT('Ctrl Pts',(12.3256628518316,58.5416666666667,-46.));
#11903=CARTESIAN_POINT('Ctrl Pts',(23.,58.3333333333333,-39.8371685740842));
#11904=CARTESIAN_POINT('Ctrl Pts',(33.6743371481683,58.125,-33.6743371481684));
#11905=CARTESIAN_POINT('Ctrl Pts',(39.8371685740842,57.9166666666667,-23.));
#11906=CARTESIAN_POINT('Ctrl Pts',(46.,57.7083333333333,-12.3256628518317));
#11907=CARTESIAN_POINT('Ctrl Pts',(46.,57.5,-5.63337527607782E-15));
#11908=CARTESIAN_POINT('Ctrl Pts',(46.,57.2916666666667,12.3256628518316));
#11909=CARTESIAN_POINT('Ctrl Pts',(39.8371685740842,57.0833333333333,23.));
#11910=CARTESIAN_POINT('Ctrl Pts',(33.6743371481684,56.875,33.6743371481683));
#11911=CARTESIAN_POINT('Ctrl Pts',(23.,56.6666666666667,39.8371685740842));
#11912=CARTESIAN_POINT('Ctrl Pts',(12.3256628518317,56.4583333333333,46.));
#11913=CARTESIAN_POINT('Ctrl Pts',(8.45006291411674E-15,56.25,46.));
#11914=CARTESIAN_POINT('Ctrl Pts',(-12.3256628518316,56.0416666666667,46.));
#11915=CARTESIAN_POINT('Ctrl Pts',(-23.,55.8333333333333,39.8371685740842));
#11916=CARTESIAN_POINT('Ctrl Pts',(-33.6743371481683,55.625,33.6743371481684));
#11917=CARTESIAN_POINT('Ctrl Pts',(-39.8371685740842,55.4166666666667,23.));
#11918=CARTESIAN_POINT('Ctrl Pts',(-46.,55.2083333333333,12.3256628518317));
#11919=CARTESIAN_POINT('Ctrl Pts',(-46.,55.,0.));
#11920=CARTESIAN_POINT('Ctrl Pts',(-46.,54.7916666666667,-12.3256628518316));
#11921=CARTESIAN_POINT('Ctrl Pts',(-39.8371685740842,54.5833333333333,-23.));
#11922=CARTESIAN_POINT('Ctrl Pts',(-33.6743371481684,54.375,-33.6743371481684));
#11923=CARTESIAN_POINT('Ctrl Pts',(-23.,54.1666666666667,-39.8371685740842));
#11924=CARTESIAN_POINT('Ctrl Pts',(-12.3256628518317,53.9583333333333,-46.));
#11925=CARTESIAN_POINT('Ctrl Pts',(-2.81668763803891E-15,53.75,-46.));
#11926=CARTESIAN_POINT('Ctrl Pts',(12.3256628518316,53.5416666666667,-46.));
#11927=CARTESIAN_POINT('Ctrl Pts',(23.,53.3333333333333,-39.8371685740842));
#11928=CARTESIAN_POINT('Ctrl Pts',(33.6743371481683,53.125,-33.6743371481684));
#11929=CARTESIAN_POINT('Ctrl Pts',(39.8371685740842,52.9166666666667,-23.));
#11930=CARTESIAN_POINT('Ctrl Pts',(46.,52.7083333333333,-12.3256628518317));
#11931=CARTESIAN_POINT('Ctrl Pts',(46.,52.5,-5.63337527607782E-15));
#11932=CARTESIAN_POINT('Ctrl Pts',(46.,52.2916666666667,12.3256628518316));
#11933=CARTESIAN_POINT('Ctrl Pts',(39.8371685740842,52.0833333333333,23.));
#11934=CARTESIAN_POINT('Ctrl Pts',(33.6743371481684,51.875,33.6743371481683));
#11935=CARTESIAN_POINT('Ctrl Pts',(23.,51.6666666666667,39.8371685740842));
#11936=CARTESIAN_POINT('Ctrl Pts',(12.3256628518317,51.4583333333333,46.));
#11937=CARTESIAN_POINT('Ctrl Pts',(8.45006291411674E-15,51.25,46.));
#11938=CARTESIAN_POINT('Ctrl Pts',(-12.3256628518316,51.0416666666667,46.));
#11939=CARTESIAN_POINT('Ctrl Pts',(-23.,50.8333333333333,39.8371685740842));
#11940=CARTESIAN_POINT('Ctrl Pts',(-33.6743371481683,50.625,33.6743371481684));
#11941=CARTESIAN_POINT('Ctrl Pts',(-39.8371685740842,50.4166666666667,23.));
#11942=CARTESIAN_POINT('Ctrl Pts',(-46.,50.2083333333333,12.3256628518317));
#11943=CARTESIAN_POINT('Ctrl Pts',(-46.,50.,0.));
#11944=CARTESIAN_POINT('Ctrl Pts',(-46.,49.7916666666667,-12.3256628518316));
#11945=CARTESIAN_POINT('Ctrl Pts',(-39.8371685740842,49.5833333333333,-23.));
#11946=CARTESIAN_POINT('Ctrl Pts',(-33.6743371481684,49.375,-33.6743371481684));
#11947=CARTESIAN_POINT('Ctrl Pts',(-23.,49.1666666666667,-39.8371685740842));
#11948=CARTESIAN_POINT('Ctrl Pts',(-12.3256628518317,48.9583333333333,-46.));
#11949=CARTESIAN_POINT('Ctrl Pts',(-2.81668763803891E-15,48.75,-46.));
#11950=CARTESIAN_POINT('Ctrl Pts',(12.3256628518316,48.5416666666667,-46.));
#11951=CARTESIAN_POINT('Ctrl Pts',(23.,48.3333333333333,-39.8371685740842));
#11952=CARTESIAN_POINT('Ctrl Pts',(33.6743371481683,48.125,-33.6743371481684));
#11953=CARTESIAN_POINT('Ctrl Pts',(39.8371685740842,47.9166666666667,-23.));
#11954=CARTESIAN_POINT('Ctrl Pts',(46.,47.7083333333333,-12.3256628518317));
#11955=CARTESIAN_POINT('Ctrl Pts',(46.,47.5,-5.63337527607782E-15));
#11956=CARTESIAN_POINT('Ctrl Pts',(46.,47.2916666666667,12.3256628518316));
#11957=CARTESIAN_POINT('Ctrl Pts',(39.8371685740842,47.0833333333333,23.));
#11958=CARTESIAN_POINT('Ctrl Pts',(33.6743371481684,46.875,33.6743371481683));
#11959=CARTESIAN_POINT('Ctrl Pts',(23.,46.6666666666667,39.8371685740842));
#11960=CARTESIAN_POINT('Ctrl Pts',(12.3256628518317,46.4583333333333,46.));
#11961=CARTESIAN_POINT('Ctrl Pts',(8.45006291411674E-15,46.25,46.));
#11962=CARTESIAN_POINT('Ctrl Pts',(-12.3256628518316,46.0416666666667,46.));
#11963=CARTESIAN_POINT('Ctrl Pts',(-23.,45.8333333333333,39.8371685740842));
#11964=CARTESIAN_POINT('Ctrl Pts',(-33.6743371481683,45.625,33.6743371481684));
#11965=CARTESIAN_POINT('Ctrl Pts',(-39.8371685740842,45.4166666666667,23.));
#11966=CARTESIAN_POINT('Ctrl Pts',(-46.,45.2083333333333,12.3256628518317));
#11967=CARTESIAN_POINT('Ctrl Pts',(-46.,45.,0.));
#11968=CARTESIAN_POINT('Ctrl Pts',(-46.,44.7916666666667,-12.3256628518316));
#11969=CARTESIAN_POINT('Ctrl Pts',(-39.8371685740842,44.5833333333333,-23.));
#11970=CARTESIAN_POINT('Ctrl Pts',(-33.6743371481684,44.375,-33.6743371481684));
#11971=CARTESIAN_POINT('Ctrl Pts',(-23.,44.1666666666667,-39.8371685740842));
#11972=CARTESIAN_POINT('Ctrl Pts',(-12.3256628518317,43.9583333333333,-46.));
#11973=CARTESIAN_POINT('Ctrl Pts',(-2.81668763803891E-15,43.75,-46.));
#11974=CARTESIAN_POINT('Ctrl Pts',(12.3256628518316,43.5416666666667,-46.));
#11975=CARTESIAN_POINT('Ctrl Pts',(23.,43.3333333333333,-39.8371685740842));
#11976=CARTESIAN_POINT('Ctrl Pts',(33.6743371481683,43.125,-33.6743371481684));
#11977=CARTESIAN_POINT('Ctrl Pts',(39.8371685740842,42.9166666666667,-23.));
#11978=CARTESIAN_POINT('Ctrl Pts',(46.,42.7083333333333,-12.3256628518317));
#11979=CARTESIAN_POINT('Ctrl Pts',(46.,42.5,-5.63337527607782E-15));
#11980=CARTESIAN_POINT('Ctrl Pts',(46.,42.2916666666667,12.3256628518316));
#11981=CARTESIAN_POINT('Ctrl Pts',(39.8371685740842,42.0833333333333,23.));
#11982=CARTESIAN_POINT('Ctrl Pts',(33.6743371481684,41.875,33.6743371481683));
#11983=CARTESIAN_POINT('Ctrl Pts',(23.,41.6666666666667,39.8371685740842));
#11984=CARTESIAN_POINT('Ctrl Pts',(12.3256628518317,41.4583333333333,46.));
#11985=CARTESIAN_POINT('Ctrl Pts',(8.45006291411674E-15,41.25,46.));
#11986=CARTESIAN_POINT('Ctrl Pts',(-12.3256628518316,41.0416666666667,46.));
#11987=CARTESIAN_POINT('Ctrl Pts',(-23.,40.8333333333333,39.8371685740842));
#11988=CARTESIAN_POINT('Ctrl Pts',(-33.6743371481683,40.625,33.6743371481684));
#11989=CARTESIAN_POINT('Ctrl Pts',(-39.8371685740842,40.4166666666667,23.));
#11990=CARTESIAN_POINT('Ctrl Pts',(-46.,40.2083333333333,12.3256628518317));
#11991=CARTESIAN_POINT('Ctrl Pts',(-46.,40.,0.));
#11992=CARTESIAN_POINT('Ctrl Pts',(-46.,39.7916666666667,-12.3256628518316));
#11993=CARTESIAN_POINT('Ctrl Pts',(-39.8371685740842,39.5833333333333,-23.));
#11994=CARTESIAN_POINT('Ctrl Pts',(-33.6743371481684,39.375,-33.6743371481684));
#11995=CARTESIAN_POINT('Ctrl Pts',(-23.,39.1666666666667,-39.8371685740842));
#11996=CARTESIAN_POINT('Ctrl Pts',(-12.3256628518317,38.9583333333333,-46.));
#11997=CARTESIAN_POINT('Ctrl Pts',(-2.81668763803891E-15,38.75,-46.));
#11998=CARTESIAN_POINT('Ctrl Pts',(12.3256628518316,38.5416666666667,-46.));
#11999=CARTESIAN_POINT('Ctrl Pts',(23.,38.3333333333333,-39.8371685740842));
#12000=CARTESIAN_POINT('Ctrl Pts',(33.6743371481683,38.125,-33.6743371481684));
#12001=CARTESIAN_POINT('Ctrl Pts',(39.8371685740842,37.9166666666667,-23.));
#12002=CARTESIAN_POINT('Ctrl Pts',(46.,37.7083333333333,-12.3256628518317));
#12003=CARTESIAN_POINT('Ctrl Pts',(46.,37.5,-5.63337527607782E-15));
#12004=CARTESIAN_POINT('Ctrl Pts',(46.,37.2916666666667,12.3256628518316));
#12005=CARTESIAN_POINT('Ctrl Pts',(39.8371685740842,37.0833333333333,23.));
#12006=CARTESIAN_POINT('Ctrl Pts',(33.6743371481684,36.875,33.6743371481683));
#12007=CARTESIAN_POINT('Ctrl Pts',(23.,36.6666666666667,39.8371685740842));
#12008=CARTESIAN_POINT('Ctrl Pts',(12.3256628518317,36.4583333333333,46.));
#12009=CARTESIAN_POINT('Ctrl Pts',(8.45006291411674E-15,36.25,46.));
#12010=CARTESIAN_POINT('Ctrl Pts',(-12.3256628518316,36.0416666666667,46.));
#12011=CARTESIAN_POINT('Ctrl Pts',(-23.,35.8333333333333,39.8371685740842));
#12012=CARTESIAN_POINT('Ctrl Pts',(-33.6743371481683,35.625,33.6743371481684));
#12013=CARTESIAN_POINT('Ctrl Pts',(-39.8371685740842,35.4166666666667,23.));
#12014=CARTESIAN_POINT('Ctrl Pts',(-46.,35.2083333333333,12.3256628518317));
#12015=CARTESIAN_POINT('Ctrl Pts',(-46.,35.,0.));
#12016=CARTESIAN_POINT('Ctrl Pts',(-46.,34.7916666666667,-12.3256628518316));
#12017=CARTESIAN_POINT('Ctrl Pts',(-39.8371685740842,34.5833333333333,-23.));
#12018=CARTESIAN_POINT('Ctrl Pts',(-33.6743371481684,34.375,-33.6743371481684));
#12019=CARTESIAN_POINT('Ctrl Pts',(-23.,34.1666666666667,-39.8371685740842));
#12020=CARTESIAN_POINT('Ctrl Pts',(-12.3256628518317,33.9583333333333,-46.));
#12021=CARTESIAN_POINT('Ctrl Pts',(-2.81668763803891E-15,33.75,-46.));
#12022=CARTESIAN_POINT('Ctrl Pts',(12.3256628518316,33.5416666666667,-46.));
#12023=CARTESIAN_POINT('Ctrl Pts',(23.,33.3333333333333,-39.8371685740842));
#12024=CARTESIAN_POINT('Ctrl Pts',(33.6743371481683,33.125,-33.6743371481684));
#12025=CARTESIAN_POINT('Ctrl Pts',(39.8371685740842,32.9166666666667,-23.));
#12026=CARTESIAN_POINT('Ctrl Pts',(46.,32.7083333333333,-12.3256628518317));
#12027=CARTESIAN_POINT('Ctrl Pts',(46.,32.5,-5.63337527607782E-15));
#12028=CARTESIAN_POINT('Ctrl Pts',(46.,32.2916666666667,12.3256628518316));
#12029=CARTESIAN_POINT('Ctrl Pts',(39.8371685740842,32.0833333333333,23.));
#12030=CARTESIAN_POINT('Ctrl Pts',(33.6743371481684,31.875,33.6743371481683));
#12031=CARTESIAN_POINT('Ctrl Pts',(23.,31.6666666666667,39.8371685740842));
#12032=CARTESIAN_POINT('Ctrl Pts',(12.3256628518317,31.4583333333333,46.));
#12033=CARTESIAN_POINT('Ctrl Pts',(8.45006291411674E-15,31.25,46.));
#12034=CARTESIAN_POINT('Ctrl Pts',(-12.3256628518316,31.0416666666667,46.));
#12035=CARTESIAN_POINT('Ctrl Pts',(-23.,30.8333333333333,39.8371685740842));
#12036=CARTESIAN_POINT('Ctrl Pts',(-33.6743371481683,30.625,33.6743371481684));
#12037=CARTESIAN_POINT('Ctrl Pts',(-39.8371685740842,30.4166666666667,23.));
#12038=CARTESIAN_POINT('Ctrl Pts',(-46.,30.2083333333333,12.3256628518317));
#12039=CARTESIAN_POINT('Ctrl Pts',(-46.,30.,0.));
#12040=CARTESIAN_POINT('Ctrl Pts',(45.7957082162897,52.5741208584476,-4.33048599679672));
#12041=CARTESIAN_POINT('Ctrl Pts',(46.027322302781,52.4406160752063,-4.33048599679672));
#12042=CARTESIAN_POINT('Ctrl Pts',(46.4905476657728,52.1736016336912,-4.33048599679677));
#12043=CARTESIAN_POINT('Ctrl Pts',(46.9537676533565,51.9065778670208,-4.33048599679672));
#12044=CARTESIAN_POINT('Ctrl Pts',(47.6280672732221,51.5178683162597,-4.33048599679672));
#12045=CARTESIAN_POINT('Ctrl Pts',(48.0707534890442,51.2626647328764,-4.33048599679671));
#12046=CARTESIAN_POINT('Ctrl Pts',(48.5134353784344,51.0074536451604,-4.33048599679671));
#12047=CARTESIAN_POINT('Ctrl Pts',(3.612927284338,52.1292520480092,-48.5721450795008));
#12048=CARTESIAN_POINT('Ctrl Pts',(3.612927284338,52.2624339185675,-48.3403451622817));
#12049=CARTESIAN_POINT('Ctrl Pts',(3.61292728433801,52.395608829009,-48.1085412459393));
#12050=CARTESIAN_POINT('Ctrl Pts',(3.61292728433801,52.6619441142016,-47.6449250631479));
#12051=CARTESIAN_POINT('Ctrl Pts',(3.612927284338,52.7951044891727,-47.4131127965212));
#12052=CARTESIAN_POINT('Ctrl Pts',(3.612927284338,52.9282572703913,-47.1812961682826));
#12053=CARTESIAN_POINT('Ctrl Pts',(3.612927284338,53.1816295626638,-46.7401795055578));
#12054=CARTESIAN_POINT('Ctrl Pts',(3.61292728433801,53.4349743764897,-46.2990470581854));
#12055=CARTESIAN_POINT('Ctrl Pts',(3.61292728433801,53.688289262853,-45.8578974271399));
#12056=CARTESIAN_POINT('Ctrl Pts',(-48.706329375,58.437500006828,-1.8898197019151E-14));
#12057=CARTESIAN_POINT('Ctrl Pts',(-48.706329375,58.2291666734946,-13.0508216223155));
#12058=CARTESIAN_POINT('Ctrl Pts',(-42.1809185638422,58.0208333401613,-24.3531646875));
#12059=CARTESIAN_POINT('Ctrl Pts',(-35.6555077526845,57.812500006828,-35.6555077526845));
#12060=CARTESIAN_POINT('Ctrl Pts',(-24.3531646875,57.6041666734946,-42.1809185638422));
#12061=CARTESIAN_POINT('Ctrl Pts',(-13.0508216223155,57.3958333401613,-48.706329375));
#12062=CARTESIAN_POINT('Ctrl Pts',(1.59157945007855E-14,57.187500006828,
-48.706329375));
#12063=CARTESIAN_POINT('Ctrl Pts',(13.0508216223155,56.9791666734946,-48.706329375));
#12064=CARTESIAN_POINT('Ctrl Pts',(24.3531646875,56.7708333401613,-42.1809185638422));
#12065=CARTESIAN_POINT('Ctrl Pts',(35.6555077526845,56.562500006828,-35.6555077526845));
#12066=CARTESIAN_POINT('Ctrl Pts',(42.1809185638422,56.3541666734946,-24.3531646875));
#12067=CARTESIAN_POINT('Ctrl Pts',(48.706329375,56.1458333401613,-13.0508216223155));
#12068=CARTESIAN_POINT('Ctrl Pts',(48.706329375,55.937500006828,1.293339198242E-14));
#12069=CARTESIAN_POINT('Ctrl Pts',(48.706329375,55.7291666734946,13.0508216223155));
#12070=CARTESIAN_POINT('Ctrl Pts',(42.1809185638422,55.5208333401613,24.3531646875));
#12071=CARTESIAN_POINT('Ctrl Pts',(35.6555077526845,55.312500006828,35.6555077526845));
#12072=CARTESIAN_POINT('Ctrl Pts',(24.3531646875,55.1041666734946,42.1809185638422));
#12073=CARTESIAN_POINT('Ctrl Pts',(13.0508216223155,54.8958333401613,48.706329375));
#12074=CARTESIAN_POINT('Ctrl Pts',(-9.95098946405443E-15,54.687500006828,
48.706329375));
#12075=CARTESIAN_POINT('Ctrl Pts',(-13.0508216223155,54.4791666734946,48.706329375));
#12076=CARTESIAN_POINT('Ctrl Pts',(-24.3531646875,54.2708333401613,42.1809185638423));
#12077=CARTESIAN_POINT('Ctrl Pts',(-35.6555077526845,54.062500006828,35.6555077526845));
#12078=CARTESIAN_POINT('Ctrl Pts',(-42.1809185638422,53.8541666734946,24.3531646875));
#12079=CARTESIAN_POINT('Ctrl Pts',(-48.706329375,53.6458333401613,13.0508216223155));
#12080=CARTESIAN_POINT('Ctrl Pts',(-48.706329375,53.437500006828,-1.8898197019151E-14));
#12081=CARTESIAN_POINT('Ctrl Pts',(-48.706329375,53.2291666734946,-13.0508216223155));
#12082=CARTESIAN_POINT('Ctrl Pts',(-42.1809185638422,53.0208333401613,-24.3531646875));
#12083=CARTESIAN_POINT('Ctrl Pts',(-35.6555077526845,52.812500006828,-35.6555077526845));
#12084=CARTESIAN_POINT('Ctrl Pts',(-24.3531646875,52.6041666734946,-42.1809185638422));
#12085=CARTESIAN_POINT('Ctrl Pts',(-13.0508216223155,52.3958333401613,-48.706329375));
#12086=CARTESIAN_POINT('Ctrl Pts',(1.59157945007855E-14,52.187500006828,
-48.706329375));
#12087=CARTESIAN_POINT('Ctrl Pts',(13.0508216223155,51.9791666734946,-48.706329375));
#12088=CARTESIAN_POINT('Ctrl Pts',(24.3531646875,51.7708333401613,-42.1809185638422));
#12089=CARTESIAN_POINT('Ctrl Pts',(35.6555077526845,51.562500006828,-35.6555077526845));
#12090=CARTESIAN_POINT('Ctrl Pts',(42.1809185638422,51.3541666734946,-24.3531646875));
#12091=CARTESIAN_POINT('Ctrl Pts',(48.706329375,51.1458333401613,-13.0508216223155));
#12092=CARTESIAN_POINT('Ctrl Pts',(48.706329375,50.937500006828,1.293339198242E-14));
#12093=CARTESIAN_POINT('Ctrl Pts',(48.706329375,50.7291666734946,13.0508216223155));
#12094=CARTESIAN_POINT('Ctrl Pts',(42.1809185638422,50.5208333401613,24.3531646875));
#12095=CARTESIAN_POINT('Ctrl Pts',(35.6555077526845,50.312500006828,35.6555077526845));
#12096=CARTESIAN_POINT('Ctrl Pts',(24.3531646875,50.1041666734946,42.1809185638422));
#12097=CARTESIAN_POINT('Ctrl Pts',(13.0508216223155,49.8958333401613,48.706329375));
#12098=CARTESIAN_POINT('Ctrl Pts',(-9.95098946405443E-15,49.687500006828,
48.706329375));
#12099=CARTESIAN_POINT('Ctrl Pts',(-13.0508216223155,49.4791666734946,48.706329375));
#12100=CARTESIAN_POINT('Ctrl Pts',(-24.3531646875,49.2708333401613,42.1809185638423));
#12101=CARTESIAN_POINT('Ctrl Pts',(-35.6555077526845,49.062500006828,35.6555077526845));
#12102=CARTESIAN_POINT('Ctrl Pts',(-42.1809185638422,48.8541666734946,24.3531646875));
#12103=CARTESIAN_POINT('Ctrl Pts',(-48.706329375,48.6458333401613,13.0508216223155));
#12104=CARTESIAN_POINT('Ctrl Pts',(-48.706329375,48.437500006828,-1.8898197019151E-14));
#12105=CARTESIAN_POINT('Ctrl Pts',(-48.706329375,48.2291666734946,-13.0508216223155));
#12106=CARTESIAN_POINT('Ctrl Pts',(-42.1809185638422,48.0208333401613,-24.3531646875));
#12107=CARTESIAN_POINT('Ctrl Pts',(-35.6555077526845,47.812500006828,-35.6555077526845));
#12108=CARTESIAN_POINT('Ctrl Pts',(-24.3531646875,47.6041666734946,-42.1809185638422));
#12109=CARTESIAN_POINT('Ctrl Pts',(-13.0508216223155,47.3958333401613,-48.706329375));
#12110=CARTESIAN_POINT('Ctrl Pts',(1.59157945007855E-14,47.187500006828,
-48.706329375));
#12111=CARTESIAN_POINT('Ctrl Pts',(13.0508216223155,46.9791666734946,-48.706329375));
#12112=CARTESIAN_POINT('Ctrl Pts',(24.3531646875,46.7708333401613,-42.1809185638422));
#12113=CARTESIAN_POINT('Ctrl Pts',(35.6555077526845,46.562500006828,-35.6555077526845));
#12114=CARTESIAN_POINT('Ctrl Pts',(42.1809185638422,46.3541666734946,-24.3531646875));
#12115=CARTESIAN_POINT('Ctrl Pts',(48.706329375,46.1458333401613,-13.0508216223155));
#12116=CARTESIAN_POINT('Ctrl Pts',(48.706329375,45.937500006828,1.293339198242E-14));
#12117=CARTESIAN_POINT('Ctrl Pts',(48.706329375,45.7291666734946,13.0508216223155));
#12118=CARTESIAN_POINT('Ctrl Pts',(42.1809185638422,45.5208333401613,24.3531646875));
#12119=CARTESIAN_POINT('Ctrl Pts',(35.6555077526845,45.312500006828,35.6555077526845));
#12120=CARTESIAN_POINT('Ctrl Pts',(24.3531646875,45.1041666734946,42.1809185638422));
#12121=CARTESIAN_POINT('Ctrl Pts',(13.0508216223155,44.8958333401613,48.706329375));
#12122=CARTESIAN_POINT('Ctrl Pts',(-9.95098946405443E-15,44.687500006828,
48.706329375));
#12123=CARTESIAN_POINT('Ctrl Pts',(-13.0508216223155,44.4791666734946,48.706329375));
#12124=CARTESIAN_POINT('Ctrl Pts',(-24.3531646875,44.2708333401613,42.1809185638423));
#12125=CARTESIAN_POINT('Ctrl Pts',(-35.6555077526845,44.062500006828,35.6555077526845));
#12126=CARTESIAN_POINT('Ctrl Pts',(-42.1809185638422,43.8541666734946,24.3531646875));
#12127=CARTESIAN_POINT('Ctrl Pts',(-48.706329375,43.6458333401613,13.0508216223155));
#12128=CARTESIAN_POINT('Ctrl Pts',(-48.706329375,43.437500006828,-1.8898197019151E-14));
#12129=CARTESIAN_POINT('Ctrl Pts',(-48.706329375,43.2291666734946,-13.0508216223155));
#12130=CARTESIAN_POINT('Ctrl Pts',(-42.1809185638422,43.0208333401613,-24.3531646875));
#12131=CARTESIAN_POINT('Ctrl Pts',(-35.6555077526845,42.812500006828,-35.6555077526845));
#12132=CARTESIAN_POINT('Ctrl Pts',(-24.3531646875,42.6041666734946,-42.1809185638422));
#12133=CARTESIAN_POINT('Ctrl Pts',(-13.0508216223155,42.3958333401613,-48.706329375));
#12134=CARTESIAN_POINT('Ctrl Pts',(1.59157945007855E-14,42.187500006828,
-48.706329375));
#12135=CARTESIAN_POINT('Ctrl Pts',(13.0508216223155,41.9791666734946,-48.706329375));
#12136=CARTESIAN_POINT('Ctrl Pts',(24.3531646875,41.7708333401613,-42.1809185638422));
#12137=CARTESIAN_POINT('Ctrl Pts',(35.6555077526845,41.562500006828,-35.6555077526845));
#12138=CARTESIAN_POINT('Ctrl Pts',(42.1809185638422,41.3541666734946,-24.3531646875));
#12139=CARTESIAN_POINT('Ctrl Pts',(48.706329375,41.1458333401613,-13.0508216223155));
#12140=CARTESIAN_POINT('Ctrl Pts',(48.706329375,40.937500006828,1.293339198242E-14));
#12141=CARTESIAN_POINT('Ctrl Pts',(48.706329375,40.7291666734946,13.0508216223155));
#12142=CARTESIAN_POINT('Ctrl Pts',(42.1809185638422,40.5208333401613,24.3531646875));
#12143=CARTESIAN_POINT('Ctrl Pts',(35.6555077526845,40.312500006828,35.6555077526845));
#12144=CARTESIAN_POINT('Ctrl Pts',(24.3531646875,40.1041666734946,42.1809185638422));
#12145=CARTESIAN_POINT('Ctrl Pts',(13.0508216223155,39.8958333401613,48.706329375));
#12146=CARTESIAN_POINT('Ctrl Pts',(-9.95098946405443E-15,39.687500006828,
48.706329375));
#12147=CARTESIAN_POINT('Ctrl Pts',(-13.0508216223155,39.4791666734946,48.706329375));
#12148=CARTESIAN_POINT('Ctrl Pts',(-24.3531646875,39.2708333401613,42.1809185638423));
#12149=CARTESIAN_POINT('Ctrl Pts',(-35.6555077526845,39.062500006828,35.6555077526845));
#12150=CARTESIAN_POINT('Ctrl Pts',(-42.1809185638422,38.8541666734946,24.3531646875));
#12151=CARTESIAN_POINT('Ctrl Pts',(-48.706329375,38.6458333401613,13.0508216223155));
#12152=CARTESIAN_POINT('Ctrl Pts',(-48.706329375,38.437500006828,-1.8898197019151E-14));
#12153=CARTESIAN_POINT('Ctrl Pts',(-48.706329375,38.2291666734946,-13.0508216223155));
#12154=CARTESIAN_POINT('Ctrl Pts',(-42.1809185638422,38.0208333401613,-24.3531646875));
#12155=CARTESIAN_POINT('Ctrl Pts',(-35.6555077526845,37.812500006828,-35.6555077526845));
#12156=CARTESIAN_POINT('Ctrl Pts',(-24.3531646875,37.6041666734946,-42.1809185638422));
#12157=CARTESIAN_POINT('Ctrl Pts',(-13.0508216223155,37.3958333401613,-48.706329375));
#12158=CARTESIAN_POINT('Ctrl Pts',(1.59157945007855E-14,37.187500006828,
-48.706329375));
#12159=CARTESIAN_POINT('Ctrl Pts',(13.0508216223155,36.9791666734946,-48.706329375));
#12160=CARTESIAN_POINT('Ctrl Pts',(24.3531646875,36.7708333401613,-42.1809185638422));
#12161=CARTESIAN_POINT('Ctrl Pts',(35.6555077526845,36.562500006828,-35.6555077526845));
#12162=CARTESIAN_POINT('Ctrl Pts',(42.1809185638422,36.3541666734946,-24.3531646875));
#12163=CARTESIAN_POINT('Ctrl Pts',(48.706329375,36.1458333401613,-13.0508216223155));
#12164=CARTESIAN_POINT('Ctrl Pts',(48.706329375,35.937500006828,1.293339198242E-14));
#12165=CARTESIAN_POINT('Ctrl Pts',(48.706329375,35.7291666734946,13.0508216223155));
#12166=CARTESIAN_POINT('Ctrl Pts',(42.1809185638422,35.5208333401613,24.3531646875));
#12167=CARTESIAN_POINT('Ctrl Pts',(35.6555077526845,35.312500006828,35.6555077526845));
#12168=CARTESIAN_POINT('Ctrl Pts',(24.3531646875,35.1041666734946,42.1809185638422));
#12169=CARTESIAN_POINT('Ctrl Pts',(13.0508216223155,34.8958333401613,48.706329375));
#12170=CARTESIAN_POINT('Ctrl Pts',(-9.95098946405443E-15,34.687500006828,
48.706329375));
#12171=CARTESIAN_POINT('Ctrl Pts',(-13.0508216223155,34.4791666734946,48.706329375));
#12172=CARTESIAN_POINT('Ctrl Pts',(-24.3531646875,34.2708333401613,42.1809185638423));
#12173=CARTESIAN_POINT('Ctrl Pts',(-35.6555077526845,34.062500006828,35.6555077526845));
#12174=CARTESIAN_POINT('Ctrl Pts',(-42.1809185638422,33.8541666734946,24.3531646875));
#12175=CARTESIAN_POINT('Ctrl Pts',(-48.706329375,33.6458333401613,13.0508216223155));
#12176=CARTESIAN_POINT('Ctrl Pts',(-48.706329375,33.437500006828,-1.8898197019151E-14));
#12177=CARTESIAN_POINT('Ctrl Pts',(-48.706329375,33.2291666734946,-13.0508216223155));
#12178=CARTESIAN_POINT('Ctrl Pts',(-42.1809185638422,33.0208333401613,-24.3531646875));
#12179=CARTESIAN_POINT('Ctrl Pts',(-35.6555077526845,32.812500006828,-35.6555077526845));
#12180=CARTESIAN_POINT('Ctrl Pts',(-24.3531646875,32.6041666734946,-42.1809185638422));
#12181=CARTESIAN_POINT('Ctrl Pts',(-13.0508216223155,32.3958333401613,-48.706329375));
#12182=CARTESIAN_POINT('Ctrl Pts',(1.59157945007855E-14,32.187500006828,
-48.706329375));
#12183=CARTESIAN_POINT('Ctrl Pts',(13.0508216223155,31.9791666734946,-48.706329375));
#12184=CARTESIAN_POINT('Ctrl Pts',(24.3531646875,31.7708333401613,-42.1809185638422));
#12185=CARTESIAN_POINT('Ctrl Pts',(35.6555077526845,31.562500006828,-35.6555077526845));
#12186=CARTESIAN_POINT('Ctrl Pts',(42.1809185638422,31.3541666734946,-24.3531646875));
#12187=CARTESIAN_POINT('Ctrl Pts',(48.706329375,31.1458333401613,-13.0508216223155));
#12188=CARTESIAN_POINT('Ctrl Pts',(48.706329375,30.937500006828,1.293339198242E-14));
#12189=CARTESIAN_POINT('Ctrl Pts',(48.706329375,30.7291666734946,13.0508216223155));
#12190=CARTESIAN_POINT('Ctrl Pts',(42.1809185638422,30.5208333401613,24.3531646875));
#12191=CARTESIAN_POINT('Ctrl Pts',(35.6555077526845,30.312500006828,35.6555077526845));
#12192=CARTESIAN_POINT('Ctrl Pts',(24.3531646875,30.1041666734946,42.1809185638422));
#12193=CARTESIAN_POINT('Ctrl Pts',(13.0508216223155,29.8958333401613,48.706329375));
#12194=CARTESIAN_POINT('Ctrl Pts',(-9.95098946405443E-15,29.687500006828,
48.706329375));
#12195=CARTESIAN_POINT('Ctrl Pts',(-13.0508216223155,29.4791666734946,48.706329375));
#12196=CARTESIAN_POINT('Ctrl Pts',(-24.3531646875,29.2708333401613,42.1809185638423));
#12197=CARTESIAN_POINT('Ctrl Pts',(-35.6555077526845,29.062500006828,35.6555077526845));
#12198=CARTESIAN_POINT('Ctrl Pts',(-42.1809185638422,28.8541666734946,24.3531646875));
#12199=CARTESIAN_POINT('Ctrl Pts',(-48.706329375,28.6458333401613,13.0508216223155));
#12200=CARTESIAN_POINT('Ctrl Pts',(-48.706329375,28.437500006828,-1.8898197019151E-14));
#12201=CARTESIAN_POINT('Ctrl Pts',(-46.,60.,0.));
#12202=CARTESIAN_POINT('Ctrl Pts',(-46.,59.7916666666667,-12.3256628518316));
#12203=CARTESIAN_POINT('Ctrl Pts',(-39.8371685740842,59.5833333333333,-23.));
#12204=CARTESIAN_POINT('Ctrl Pts',(-33.6743371481684,59.375,-33.6743371481684));
#12205=CARTESIAN_POINT('Ctrl Pts',(-23.,59.1666666666667,-39.8371685740842));
#12206=CARTESIAN_POINT('Ctrl Pts',(-12.3256628518317,58.9583333333333,-46.));
#12207=CARTESIAN_POINT('Ctrl Pts',(-2.81668763803891E-15,58.75,-46.));
#12208=CARTESIAN_POINT('Ctrl Pts',(12.3256628518316,58.5416666666667,-46.));
#12209=CARTESIAN_POINT('Ctrl Pts',(23.,58.3333333333333,-39.8371685740842));
#12210=CARTESIAN_POINT('Ctrl Pts',(33.6743371481683,58.125,-33.6743371481684));
#12211=CARTESIAN_POINT('Ctrl Pts',(39.8371685740842,57.9166666666667,-23.));
#12212=CARTESIAN_POINT('Ctrl Pts',(46.,57.7083333333333,-12.3256628518317));
#12213=CARTESIAN_POINT('Ctrl Pts',(46.,57.5,-5.63337527607782E-15));
#12214=CARTESIAN_POINT('Ctrl Pts',(46.,57.2916666666667,12.3256628518316));
#12215=CARTESIAN_POINT('Ctrl Pts',(39.8371685740842,57.0833333333333,23.));
#12216=CARTESIAN_POINT('Ctrl Pts',(33.6743371481684,56.875,33.6743371481683));
#12217=CARTESIAN_POINT('Ctrl Pts',(23.,56.6666666666667,39.8371685740842));
#12218=CARTESIAN_POINT('Ctrl Pts',(12.3256628518317,56.4583333333333,46.));
#12219=CARTESIAN_POINT('Ctrl Pts',(8.45006291411674E-15,56.25,46.));
#12220=CARTESIAN_POINT('Ctrl Pts',(-12.3256628518316,56.0416666666667,46.));
#12221=CARTESIAN_POINT('Ctrl Pts',(-23.,55.8333333333333,39.8371685740842));
#12222=CARTESIAN_POINT('Ctrl Pts',(-33.6743371481683,55.625,33.6743371481684));
#12223=CARTESIAN_POINT('Ctrl Pts',(-39.8371685740842,55.4166666666667,23.));
#12224=CARTESIAN_POINT('Ctrl Pts',(-46.,55.2083333333333,12.3256628518317));
#12225=CARTESIAN_POINT('Ctrl Pts',(-46.,55.,0.));
#12226=CARTESIAN_POINT('Ctrl Pts',(-46.,54.7916666666667,-12.3256628518316));
#12227=CARTESIAN_POINT('Ctrl Pts',(-39.8371685740842,54.5833333333333,-23.));
#12228=CARTESIAN_POINT('Ctrl Pts',(-33.6743371481684,54.375,-33.6743371481684));
#12229=CARTESIAN_POINT('Ctrl Pts',(-23.,54.1666666666667,-39.8371685740842));
#12230=CARTESIAN_POINT('Ctrl Pts',(-12.3256628518317,53.9583333333333,-46.));
#12231=CARTESIAN_POINT('Ctrl Pts',(-2.81668763803891E-15,53.75,-46.));
#12232=CARTESIAN_POINT('Ctrl Pts',(12.3256628518316,53.5416666666667,-46.));
#12233=CARTESIAN_POINT('Ctrl Pts',(23.,53.3333333333333,-39.8371685740842));
#12234=CARTESIAN_POINT('Ctrl Pts',(33.6743371481683,53.125,-33.6743371481684));
#12235=CARTESIAN_POINT('Ctrl Pts',(39.8371685740842,52.9166666666667,-23.));
#12236=CARTESIAN_POINT('Ctrl Pts',(46.,52.7083333333333,-12.3256628518317));
#12237=CARTESIAN_POINT('Ctrl Pts',(46.,52.5,-5.63337527607782E-15));
#12238=CARTESIAN_POINT('Ctrl Pts',(46.,52.2916666666667,12.3256628518316));
#12239=CARTESIAN_POINT('Ctrl Pts',(39.8371685740842,52.0833333333333,23.));
#12240=CARTESIAN_POINT('Ctrl Pts',(33.6743371481684,51.875,33.6743371481683));
#12241=CARTESIAN_POINT('Ctrl Pts',(23.,51.6666666666667,39.8371685740842));
#12242=CARTESIAN_POINT('Ctrl Pts',(12.3256628518317,51.4583333333333,46.));
#12243=CARTESIAN_POINT('Ctrl Pts',(8.45006291411674E-15,51.25,46.));
#12244=CARTESIAN_POINT('Ctrl Pts',(-12.3256628518316,51.0416666666667,46.));
#12245=CARTESIAN_POINT('Ctrl Pts',(-23.,50.8333333333333,39.8371685740842));
#12246=CARTESIAN_POINT('Ctrl Pts',(-33.6743371481683,50.625,33.6743371481684));
#12247=CARTESIAN_POINT('Ctrl Pts',(-39.8371685740842,50.4166666666667,23.));
#12248=CARTESIAN_POINT('Ctrl Pts',(-46.,50.2083333333333,12.3256628518317));
#12249=CARTESIAN_POINT('Ctrl Pts',(-46.,50.,0.));
#12250=CARTESIAN_POINT('Ctrl Pts',(-46.,49.7916666666667,-12.3256628518316));
#12251=CARTESIAN_POINT('Ctrl Pts',(-39.8371685740842,49.5833333333333,-23.));
#12252=CARTESIAN_POINT('Ctrl Pts',(-33.6743371481684,49.375,-33.6743371481684));
#12253=CARTESIAN_POINT('Ctrl Pts',(-23.,49.1666666666667,-39.8371685740842));
#12254=CARTESIAN_POINT('Ctrl Pts',(-12.3256628518317,48.9583333333333,-46.));
#12255=CARTESIAN_POINT('Ctrl Pts',(-2.81668763803891E-15,48.75,-46.));
#12256=CARTESIAN_POINT('Ctrl Pts',(12.3256628518316,48.5416666666667,-46.));
#12257=CARTESIAN_POINT('Ctrl Pts',(23.,48.3333333333333,-39.8371685740842));
#12258=CARTESIAN_POINT('Ctrl Pts',(33.6743371481683,48.125,-33.6743371481684));
#12259=CARTESIAN_POINT('Ctrl Pts',(39.8371685740842,47.9166666666667,-23.));
#12260=CARTESIAN_POINT('Ctrl Pts',(46.,47.7083333333333,-12.3256628518317));
#12261=CARTESIAN_POINT('Ctrl Pts',(46.,47.5,-5.63337527607782E-15));
#12262=CARTESIAN_POINT('Ctrl Pts',(46.,47.2916666666667,12.3256628518316));
#12263=CARTESIAN_POINT('Ctrl Pts',(39.8371685740842,47.0833333333333,23.));
#12264=CARTESIAN_POINT('Ctrl Pts',(33.6743371481684,46.875,33.6743371481683));
#12265=CARTESIAN_POINT('Ctrl Pts',(23.,46.6666666666667,39.8371685740842));
#12266=CARTESIAN_POINT('Ctrl Pts',(12.3256628518317,46.4583333333333,46.));
#12267=CARTESIAN_POINT('Ctrl Pts',(8.45006291411674E-15,46.25,46.));
#12268=CARTESIAN_POINT('Ctrl Pts',(-12.3256628518316,46.0416666666667,46.));
#12269=CARTESIAN_POINT('Ctrl Pts',(-23.,45.8333333333333,39.8371685740842));
#12270=CARTESIAN_POINT('Ctrl Pts',(-33.6743371481683,45.625,33.6743371481684));
#12271=CARTESIAN_POINT('Ctrl Pts',(-39.8371685740842,45.4166666666667,23.));
#12272=CARTESIAN_POINT('Ctrl Pts',(-46.,45.2083333333333,12.3256628518317));
#12273=CARTESIAN_POINT('Ctrl Pts',(-46.,45.,0.));
#12274=CARTESIAN_POINT('Ctrl Pts',(-46.,44.7916666666667,-12.3256628518316));
#12275=CARTESIAN_POINT('Ctrl Pts',(-39.8371685740842,44.5833333333333,-23.));
#12276=CARTESIAN_POINT('Ctrl Pts',(-33.6743371481684,44.375,-33.6743371481684));
#12277=CARTESIAN_POINT('Ctrl Pts',(-23.,44.1666666666667,-39.8371685740842));
#12278=CARTESIAN_POINT('Ctrl Pts',(-12.3256628518317,43.9583333333333,-46.));
#12279=CARTESIAN_POINT('Ctrl Pts',(-2.81668763803891E-15,43.75,-46.));
#12280=CARTESIAN_POINT('Ctrl Pts',(12.3256628518316,43.5416666666667,-46.));
#12281=CARTESIAN_POINT('Ctrl Pts',(23.,43.3333333333333,-39.8371685740842));
#12282=CARTESIAN_POINT('Ctrl Pts',(33.6743371481683,43.125,-33.6743371481684));
#12283=CARTESIAN_POINT('Ctrl Pts',(39.8371685740842,42.9166666666667,-23.));
#12284=CARTESIAN_POINT('Ctrl Pts',(46.,42.7083333333333,-12.3256628518317));
#12285=CARTESIAN_POINT('Ctrl Pts',(46.,42.5,-5.63337527607782E-15));
#12286=CARTESIAN_POINT('Ctrl Pts',(46.,42.2916666666667,12.3256628518316));
#12287=CARTESIAN_POINT('Ctrl Pts',(39.8371685740842,42.0833333333333,23.));
#12288=CARTESIAN_POINT('Ctrl Pts',(33.6743371481684,41.875,33.6743371481683));
#12289=CARTESIAN_POINT('Ctrl Pts',(23.,41.6666666666667,39.8371685740842));
#12290=CARTESIAN_POINT('Ctrl Pts',(12.3256628518317,41.4583333333333,46.));
#12291=CARTESIAN_POINT('Ctrl Pts',(8.45006291411674E-15,41.25,46.));
#12292=CARTESIAN_POINT('Ctrl Pts',(-12.3256628518316,41.0416666666667,46.));
#12293=CARTESIAN_POINT('Ctrl Pts',(-23.,40.8333333333333,39.8371685740842));
#12294=CARTESIAN_POINT('Ctrl Pts',(-33.6743371481683,40.625,33.6743371481684));
#12295=CARTESIAN_POINT('Ctrl Pts',(-39.8371685740842,40.4166666666667,23.));
#12296=CARTESIAN_POINT('Ctrl Pts',(-46.,40.2083333333333,12.3256628518317));
#12297=CARTESIAN_POINT('Ctrl Pts',(-46.,40.,0.));
#12298=CARTESIAN_POINT('Ctrl Pts',(-46.,39.7916666666667,-12.3256628518316));
#12299=CARTESIAN_POINT('Ctrl Pts',(-39.8371685740842,39.5833333333333,-23.));
#12300=CARTESIAN_POINT('Ctrl Pts',(-33.6743371481684,39.375,-33.6743371481684));
#12301=CARTESIAN_POINT('Ctrl Pts',(-23.,39.1666666666667,-39.8371685740842));
#12302=CARTESIAN_POINT('Ctrl Pts',(-12.3256628518317,38.9583333333333,-46.));
#12303=CARTESIAN_POINT('Ctrl Pts',(-2.81668763803891E-15,38.75,-46.));
#12304=CARTESIAN_POINT('Ctrl Pts',(12.3256628518316,38.5416666666667,-46.));
#12305=CARTESIAN_POINT('Ctrl Pts',(23.,38.3333333333333,-39.8371685740842));
#12306=CARTESIAN_POINT('Ctrl Pts',(33.6743371481683,38.125,-33.6743371481684));
#12307=CARTESIAN_POINT('Ctrl Pts',(39.8371685740842,37.9166666666667,-23.));
#12308=CARTESIAN_POINT('Ctrl Pts',(46.,37.7083333333333,-12.3256628518317));
#12309=CARTESIAN_POINT('Ctrl Pts',(46.,37.5,-5.63337527607782E-15));
#12310=CARTESIAN_POINT('Ctrl Pts',(46.,37.2916666666667,12.3256628518316));
#12311=CARTESIAN_POINT('Ctrl Pts',(39.8371685740842,37.0833333333333,23.));
#12312=CARTESIAN_POINT('Ctrl Pts',(33.6743371481684,36.875,33.6743371481683));
#12313=CARTESIAN_POINT('Ctrl Pts',(23.,36.6666666666667,39.8371685740842));
#12314=CARTESIAN_POINT('Ctrl Pts',(12.3256628518317,36.4583333333333,46.));
#12315=CARTESIAN_POINT('Ctrl Pts',(8.45006291411674E-15,36.25,46.));
#12316=CARTESIAN_POINT('Ctrl Pts',(-12.3256628518316,36.0416666666667,46.));
#12317=CARTESIAN_POINT('Ctrl Pts',(-23.,35.8333333333333,39.8371685740842));
#12318=CARTESIAN_POINT('Ctrl Pts',(-33.6743371481683,35.625,33.6743371481684));
#12319=CARTESIAN_POINT('Ctrl Pts',(-39.8371685740842,35.4166666666667,23.));
#12320=CARTESIAN_POINT('Ctrl Pts',(-46.,35.2083333333333,12.3256628518317));
#12321=CARTESIAN_POINT('Ctrl Pts',(-46.,35.,0.));
#12322=CARTESIAN_POINT('Ctrl Pts',(-46.,34.7916666666667,-12.3256628518316));
#12323=CARTESIAN_POINT('Ctrl Pts',(-39.8371685740842,34.5833333333333,-23.));
#12324=CARTESIAN_POINT('Ctrl Pts',(-33.6743371481684,34.375,-33.6743371481684));
#12325=CARTESIAN_POINT('Ctrl Pts',(-23.,34.1666666666667,-39.8371685740842));
#12326=CARTESIAN_POINT('Ctrl Pts',(-12.3256628518317,33.9583333333333,-46.));
#12327=CARTESIAN_POINT('Ctrl Pts',(-2.81668763803891E-15,33.75,-46.));
#12328=CARTESIAN_POINT('Ctrl Pts',(12.3256628518316,33.5416666666667,-46.));
#12329=CARTESIAN_POINT('Ctrl Pts',(23.,33.3333333333333,-39.8371685740842));
#12330=CARTESIAN_POINT('Ctrl Pts',(33.6743371481683,33.125,-33.6743371481684));
#12331=CARTESIAN_POINT('Ctrl Pts',(39.8371685740842,32.9166666666667,-23.));
#12332=CARTESIAN_POINT('Ctrl Pts',(46.,32.7083333333333,-12.3256628518317));
#12333=CARTESIAN_POINT('Ctrl Pts',(46.,32.5,-5.63337527607782E-15));
#12334=CARTESIAN_POINT('Ctrl Pts',(46.,32.2916666666667,12.3256628518316));
#12335=CARTESIAN_POINT('Ctrl Pts',(39.8371685740842,32.0833333333333,23.));
#12336=CARTESIAN_POINT('Ctrl Pts',(33.6743371481684,31.875,33.6743371481683));
#12337=CARTESIAN_POINT('Ctrl Pts',(23.,31.6666666666667,39.8371685740842));
#12338=CARTESIAN_POINT('Ctrl Pts',(12.3256628518317,31.4583333333333,46.));
#12339=CARTESIAN_POINT('Ctrl Pts',(8.45006291411674E-15,31.25,46.));
#12340=CARTESIAN_POINT('Ctrl Pts',(-12.3256628518316,31.0416666666667,46.));
#12341=CARTESIAN_POINT('Ctrl Pts',(-23.,30.8333333333333,39.8371685740842));
#12342=CARTESIAN_POINT('Ctrl Pts',(-33.6743371481683,30.625,33.6743371481684));
#12343=CARTESIAN_POINT('Ctrl Pts',(-39.8371685740842,30.4166666666667,23.));
#12344=CARTESIAN_POINT('Ctrl Pts',(-46.,30.2083333333333,12.3256628518317));
#12345=CARTESIAN_POINT('Ctrl Pts',(-46.,30.,0.));
#12346=CARTESIAN_POINT('Ctrl Pts',(48.5725845633798,50.8793483229262,3.60701400320328));
#12347=CARTESIAN_POINT('Ctrl Pts',(48.3407853679392,51.0125314497137,3.60701400320328));
#12348=CARTESIAN_POINT('Ctrl Pts',(48.1089821836664,51.1457076343818,3.60701400320327));
#12349=CARTESIAN_POINT('Ctrl Pts',(47.6453674864979,51.4120455056142,3.60701400320327));
#12350=CARTESIAN_POINT('Ctrl Pts',(47.4135559734254,51.5452071923974,3.60701400320325));
#12351=CARTESIAN_POINT('Ctrl Pts',(47.1817401099609,51.6783613050641,3.60701400320325));
#12352=CARTESIAN_POINT('Ctrl Pts',(46.7406305897488,51.9317328641751,3.60701400320325));
#12353=CARTESIAN_POINT('Ctrl Pts',(46.2995053259033,52.1850770165971,3.60701400320324));
#12354=CARTESIAN_POINT('Ctrl Pts',(45.858362923034,52.438391319744,3.60701400320324));
#12355=CARTESIAN_POINT('Ctrl Pts',(3.61292728433799,51.311710737147,45.8578974271399));
#12356=CARTESIAN_POINT('Ctrl Pts',(3.61292728433798,51.178117727701,46.089460636719));
#12357=CARTESIAN_POINT('Ctrl Pts',(3.61292728433804,50.9109294856547,46.5525857733052));
#12358=CARTESIAN_POINT('Ctrl Pts',(3.61292728433797,50.6437369897944,47.0157084557285));
#12359=CARTESIAN_POINT('Ctrl Pts',(3.61292728433797,50.2553460757965,47.6888965792834));
#12360=CARTESIAN_POINT('Ctrl Pts',(3.61292728433797,50.0005487265709,48.1305218136162));
#12361=CARTESIAN_POINT('Ctrl Pts',(3.61292728433797,49.7457479656467,48.5721450795008));
#12362=CARTESIAN_POINT('Ctrl Pts',(-48.706329375,58.437500006828,-1.8898197019151E-14));
#12363=CARTESIAN_POINT('Ctrl Pts',(-48.706329375,58.2291666734946,-13.0508216223155));
#12364=CARTESIAN_POINT('Ctrl Pts',(-42.1809185638422,58.0208333401613,-24.3531646875));
#12365=CARTESIAN_POINT('Ctrl Pts',(-35.6555077526845,57.812500006828,-35.6555077526845));
#12366=CARTESIAN_POINT('Ctrl Pts',(-24.3531646875,57.6041666734946,-42.1809185638422));
#12367=CARTESIAN_POINT('Ctrl Pts',(-13.0508216223155,57.3958333401613,-48.706329375));
#12368=CARTESIAN_POINT('Ctrl Pts',(1.59157945007855E-14,57.187500006828,
-48.706329375));
#12369=CARTESIAN_POINT('Ctrl Pts',(13.0508216223155,56.9791666734946,-48.706329375));
#12370=CARTESIAN_POINT('Ctrl Pts',(24.3531646875,56.7708333401613,-42.1809185638422));
#12371=CARTESIAN_POINT('Ctrl Pts',(35.6555077526845,56.562500006828,-35.6555077526845));
#12372=CARTESIAN_POINT('Ctrl Pts',(42.1809185638422,56.3541666734946,-24.3531646875));
#12373=CARTESIAN_POINT('Ctrl Pts',(48.706329375,56.1458333401613,-13.0508216223155));
#12374=CARTESIAN_POINT('Ctrl Pts',(48.706329375,55.937500006828,1.293339198242E-14));
#12375=CARTESIAN_POINT('Ctrl Pts',(48.706329375,55.7291666734946,13.0508216223155));
#12376=CARTESIAN_POINT('Ctrl Pts',(42.1809185638422,55.5208333401613,24.3531646875));
#12377=CARTESIAN_POINT('Ctrl Pts',(35.6555077526845,55.312500006828,35.6555077526845));
#12378=CARTESIAN_POINT('Ctrl Pts',(24.3531646875,55.1041666734946,42.1809185638422));
#12379=CARTESIAN_POINT('Ctrl Pts',(13.0508216223155,54.8958333401613,48.706329375));
#12380=CARTESIAN_POINT('Ctrl Pts',(-9.95098946405443E-15,54.687500006828,
48.706329375));
#12381=CARTESIAN_POINT('Ctrl Pts',(-13.0508216223155,54.4791666734946,48.706329375));
#12382=CARTESIAN_POINT('Ctrl Pts',(-24.3531646875,54.2708333401613,42.1809185638423));
#12383=CARTESIAN_POINT('Ctrl Pts',(-35.6555077526845,54.062500006828,35.6555077526845));
#12384=CARTESIAN_POINT('Ctrl Pts',(-42.1809185638422,53.8541666734946,24.3531646875));
#12385=CARTESIAN_POINT('Ctrl Pts',(-48.706329375,53.6458333401613,13.0508216223155));
#12386=CARTESIAN_POINT('Ctrl Pts',(-48.706329375,53.437500006828,-1.8898197019151E-14));
#12387=CARTESIAN_POINT('Ctrl Pts',(-48.706329375,53.2291666734946,-13.0508216223155));
#12388=CARTESIAN_POINT('Ctrl Pts',(-42.1809185638422,53.0208333401613,-24.3531646875));
#12389=CARTESIAN_POINT('Ctrl Pts',(-35.6555077526845,52.812500006828,-35.6555077526845));
#12390=CARTESIAN_POINT('Ctrl Pts',(-24.3531646875,52.6041666734946,-42.1809185638422));
#12391=CARTESIAN_POINT('Ctrl Pts',(-13.0508216223155,52.3958333401613,-48.706329375));
#12392=CARTESIAN_POINT('Ctrl Pts',(1.59157945007855E-14,52.187500006828,
-48.706329375));
#12393=CARTESIAN_POINT('Ctrl Pts',(13.0508216223155,51.9791666734946,-48.706329375));
#12394=CARTESIAN_POINT('Ctrl Pts',(24.3531646875,51.7708333401613,-42.1809185638422));
#12395=CARTESIAN_POINT('Ctrl Pts',(35.6555077526845,51.562500006828,-35.6555077526845));
#12396=CARTESIAN_POINT('Ctrl Pts',(42.1809185638422,51.3541666734946,-24.3531646875));
#12397=CARTESIAN_POINT('Ctrl Pts',(48.706329375,51.1458333401613,-13.0508216223155));
#12398=CARTESIAN_POINT('Ctrl Pts',(48.706329375,50.937500006828,1.293339198242E-14));
#12399=CARTESIAN_POINT('Ctrl Pts',(48.706329375,50.7291666734946,13.0508216223155));
#12400=CARTESIAN_POINT('Ctrl Pts',(42.1809185638422,50.5208333401613,24.3531646875));
#12401=CARTESIAN_POINT('Ctrl Pts',(35.6555077526845,50.312500006828,35.6555077526845));
#12402=CARTESIAN_POINT('Ctrl Pts',(24.3531646875,50.1041666734946,42.1809185638422));
#12403=CARTESIAN_POINT('Ctrl Pts',(13.0508216223155,49.8958333401613,48.706329375));
#12404=CARTESIAN_POINT('Ctrl Pts',(-9.95098946405443E-15,49.687500006828,
48.706329375));
#12405=CARTESIAN_POINT('Ctrl Pts',(-13.0508216223155,49.4791666734946,48.706329375));
#12406=CARTESIAN_POINT('Ctrl Pts',(-24.3531646875,49.2708333401613,42.1809185638423));
#12407=CARTESIAN_POINT('Ctrl Pts',(-35.6555077526845,49.062500006828,35.6555077526845));
#12408=CARTESIAN_POINT('Ctrl Pts',(-42.1809185638422,48.8541666734946,24.3531646875));
#12409=CARTESIAN_POINT('Ctrl Pts',(-48.706329375,48.6458333401613,13.0508216223155));
#12410=CARTESIAN_POINT('Ctrl Pts',(-48.706329375,48.437500006828,-1.8898197019151E-14));
#12411=CARTESIAN_POINT('Ctrl Pts',(-48.706329375,48.2291666734946,-13.0508216223155));
#12412=CARTESIAN_POINT('Ctrl Pts',(-42.1809185638422,48.0208333401613,-24.3531646875));
#12413=CARTESIAN_POINT('Ctrl Pts',(-35.6555077526845,47.812500006828,-35.6555077526845));
#12414=CARTESIAN_POINT('Ctrl Pts',(-24.3531646875,47.6041666734946,-42.1809185638422));
#12415=CARTESIAN_POINT('Ctrl Pts',(-13.0508216223155,47.3958333401613,-48.706329375));
#12416=CARTESIAN_POINT('Ctrl Pts',(1.59157945007855E-14,47.187500006828,
-48.706329375));
#12417=CARTESIAN_POINT('Ctrl Pts',(13.0508216223155,46.9791666734946,-48.706329375));
#12418=CARTESIAN_POINT('Ctrl Pts',(24.3531646875,46.7708333401613,-42.1809185638422));
#12419=CARTESIAN_POINT('Ctrl Pts',(35.6555077526845,46.562500006828,-35.6555077526845));
#12420=CARTESIAN_POINT('Ctrl Pts',(42.1809185638422,46.3541666734946,-24.3531646875));
#12421=CARTESIAN_POINT('Ctrl Pts',(48.706329375,46.1458333401613,-13.0508216223155));
#12422=CARTESIAN_POINT('Ctrl Pts',(48.706329375,45.937500006828,1.293339198242E-14));
#12423=CARTESIAN_POINT('Ctrl Pts',(48.706329375,45.7291666734946,13.0508216223155));
#12424=CARTESIAN_POINT('Ctrl Pts',(42.1809185638422,45.5208333401613,24.3531646875));
#12425=CARTESIAN_POINT('Ctrl Pts',(35.6555077526845,45.312500006828,35.6555077526845));
#12426=CARTESIAN_POINT('Ctrl Pts',(24.3531646875,45.1041666734946,42.1809185638422));
#12427=CARTESIAN_POINT('Ctrl Pts',(13.0508216223155,44.8958333401613,48.706329375));
#12428=CARTESIAN_POINT('Ctrl Pts',(-9.95098946405443E-15,44.687500006828,
48.706329375));
#12429=CARTESIAN_POINT('Ctrl Pts',(-13.0508216223155,44.4791666734946,48.706329375));
#12430=CARTESIAN_POINT('Ctrl Pts',(-24.3531646875,44.2708333401613,42.1809185638423));
#12431=CARTESIAN_POINT('Ctrl Pts',(-35.6555077526845,44.062500006828,35.6555077526845));
#12432=CARTESIAN_POINT('Ctrl Pts',(-42.1809185638422,43.8541666734946,24.3531646875));
#12433=CARTESIAN_POINT('Ctrl Pts',(-48.706329375,43.6458333401613,13.0508216223155));
#12434=CARTESIAN_POINT('Ctrl Pts',(-48.706329375,43.437500006828,-1.8898197019151E-14));
#12435=CARTESIAN_POINT('Ctrl Pts',(-48.706329375,43.2291666734946,-13.0508216223155));
#12436=CARTESIAN_POINT('Ctrl Pts',(-42.1809185638422,43.0208333401613,-24.3531646875));
#12437=CARTESIAN_POINT('Ctrl Pts',(-35.6555077526845,42.812500006828,-35.6555077526845));
#12438=CARTESIAN_POINT('Ctrl Pts',(-24.3531646875,42.6041666734946,-42.1809185638422));
#12439=CARTESIAN_POINT('Ctrl Pts',(-13.0508216223155,42.3958333401613,-48.706329375));
#12440=CARTESIAN_POINT('Ctrl Pts',(1.59157945007855E-14,42.187500006828,
-48.706329375));
#12441=CARTESIAN_POINT('Ctrl Pts',(13.0508216223155,41.9791666734946,-48.706329375));
#12442=CARTESIAN_POINT('Ctrl Pts',(24.3531646875,41.7708333401613,-42.1809185638422));
#12443=CARTESIAN_POINT('Ctrl Pts',(35.6555077526845,41.562500006828,-35.6555077526845));
#12444=CARTESIAN_POINT('Ctrl Pts',(42.1809185638422,41.3541666734946,-24.3531646875));
#12445=CARTESIAN_POINT('Ctrl Pts',(48.706329375,41.1458333401613,-13.0508216223155));
#12446=CARTESIAN_POINT('Ctrl Pts',(48.706329375,40.937500006828,1.293339198242E-14));
#12447=CARTESIAN_POINT('Ctrl Pts',(48.706329375,40.7291666734946,13.0508216223155));
#12448=CARTESIAN_POINT('Ctrl Pts',(42.1809185638422,40.5208333401613,24.3531646875));
#12449=CARTESIAN_POINT('Ctrl Pts',(35.6555077526845,40.312500006828,35.6555077526845));
#12450=CARTESIAN_POINT('Ctrl Pts',(24.3531646875,40.1041666734946,42.1809185638422));
#12451=CARTESIAN_POINT('Ctrl Pts',(13.0508216223155,39.8958333401613,48.706329375));
#12452=CARTESIAN_POINT('Ctrl Pts',(-9.95098946405443E-15,39.687500006828,
48.706329375));
#12453=CARTESIAN_POINT('Ctrl Pts',(-13.0508216223155,39.4791666734946,48.706329375));
#12454=CARTESIAN_POINT('Ctrl Pts',(-24.3531646875,39.2708333401613,42.1809185638423));
#12455=CARTESIAN_POINT('Ctrl Pts',(-35.6555077526845,39.062500006828,35.6555077526845));
#12456=CARTESIAN_POINT('Ctrl Pts',(-42.1809185638422,38.8541666734946,24.3531646875));
#12457=CARTESIAN_POINT('Ctrl Pts',(-48.706329375,38.6458333401613,13.0508216223155));
#12458=CARTESIAN_POINT('Ctrl Pts',(-48.706329375,38.437500006828,-1.8898197019151E-14));
#12459=CARTESIAN_POINT('Ctrl Pts',(-48.706329375,38.2291666734946,-13.0508216223155));
#12460=CARTESIAN_POINT('Ctrl Pts',(-42.1809185638422,38.0208333401613,-24.3531646875));
#12461=CARTESIAN_POINT('Ctrl Pts',(-35.6555077526845,37.812500006828,-35.6555077526845));
#12462=CARTESIAN_POINT('Ctrl Pts',(-24.3531646875,37.6041666734946,-42.1809185638422));
#12463=CARTESIAN_POINT('Ctrl Pts',(-13.0508216223155,37.3958333401613,-48.706329375));
#12464=CARTESIAN_POINT('Ctrl Pts',(1.59157945007855E-14,37.187500006828,
-48.706329375));
#12465=CARTESIAN_POINT('Ctrl Pts',(13.0508216223155,36.9791666734946,-48.706329375));
#12466=CARTESIAN_POINT('Ctrl Pts',(24.3531646875,36.7708333401613,-42.1809185638422));
#12467=CARTESIAN_POINT('Ctrl Pts',(35.6555077526845,36.562500006828,-35.6555077526845));
#12468=CARTESIAN_POINT('Ctrl Pts',(42.1809185638422,36.3541666734946,-24.3531646875));
#12469=CARTESIAN_POINT('Ctrl Pts',(48.706329375,36.1458333401613,-13.0508216223155));
#12470=CARTESIAN_POINT('Ctrl Pts',(48.706329375,35.937500006828,1.293339198242E-14));
#12471=CARTESIAN_POINT('Ctrl Pts',(48.706329375,35.7291666734946,13.0508216223155));
#12472=CARTESIAN_POINT('Ctrl Pts',(42.1809185638422,35.5208333401613,24.3531646875));
#12473=CARTESIAN_POINT('Ctrl Pts',(35.6555077526845,35.312500006828,35.6555077526845));
#12474=CARTESIAN_POINT('Ctrl Pts',(24.3531646875,35.1041666734946,42.1809185638422));
#12475=CARTESIAN_POINT('Ctrl Pts',(13.0508216223155,34.8958333401613,48.706329375));
#12476=CARTESIAN_POINT('Ctrl Pts',(-9.95098946405443E-15,34.687500006828,
48.706329375));
#12477=CARTESIAN_POINT('Ctrl Pts',(-13.0508216223155,34.4791666734946,48.706329375));
#12478=CARTESIAN_POINT('Ctrl Pts',(-24.3531646875,34.2708333401613,42.1809185638423));
#12479=CARTESIAN_POINT('Ctrl Pts',(-35.6555077526845,34.062500006828,35.6555077526845));
#12480=CARTESIAN_POINT('Ctrl Pts',(-42.1809185638422,33.8541666734946,24.3531646875));
#12481=CARTESIAN_POINT('Ctrl Pts',(-48.706329375,33.6458333401613,13.0508216223155));
#12482=CARTESIAN_POINT('Ctrl Pts',(-48.706329375,33.437500006828,-1.8898197019151E-14));
#12483=CARTESIAN_POINT('Ctrl Pts',(-48.706329375,33.2291666734946,-13.0508216223155));
#12484=CARTESIAN_POINT('Ctrl Pts',(-42.1809185638422,33.0208333401613,-24.3531646875));
#12485=CARTESIAN_POINT('Ctrl Pts',(-35.6555077526845,32.812500006828,-35.6555077526845));
#12486=CARTESIAN_POINT('Ctrl Pts',(-24.3531646875,32.6041666734946,-42.1809185638422));
#12487=CARTESIAN_POINT('Ctrl Pts',(-13.0508216223155,32.3958333401613,-48.706329375));
#12488=CARTESIAN_POINT('Ctrl Pts',(1.59157945007855E-14,32.187500006828,
-48.706329375));
#12489=CARTESIAN_POINT('Ctrl Pts',(13.0508216223155,31.9791666734946,-48.706329375));
#12490=CARTESIAN_POINT('Ctrl Pts',(24.3531646875,31.7708333401613,-42.1809185638422));
#12491=CARTESIAN_POINT('Ctrl Pts',(35.6555077526845,31.562500006828,-35.6555077526845));
#12492=CARTESIAN_POINT('Ctrl Pts',(42.1809185638422,31.3541666734946,-24.3531646875));
#12493=CARTESIAN_POINT('Ctrl Pts',(48.706329375,31.1458333401613,-13.0508216223155));
#12494=CARTESIAN_POINT('Ctrl Pts',(48.706329375,30.937500006828,1.293339198242E-14));
#12495=CARTESIAN_POINT('Ctrl Pts',(48.706329375,30.7291666734946,13.0508216223155));
#12496=CARTESIAN_POINT('Ctrl Pts',(42.1809185638422,30.5208333401613,24.3531646875));
#12497=CARTESIAN_POINT('Ctrl Pts',(35.6555077526845,30.312500006828,35.6555077526845));
#12498=CARTESIAN_POINT('Ctrl Pts',(24.3531646875,30.1041666734946,42.1809185638422));
#12499=CARTESIAN_POINT('Ctrl Pts',(13.0508216223155,29.8958333401613,48.706329375));
#12500=CARTESIAN_POINT('Ctrl Pts',(-9.95098946405443E-15,29.687500006828,
48.706329375));
#12501=CARTESIAN_POINT('Ctrl Pts',(-13.0508216223155,29.4791666734946,48.706329375));
#12502=CARTESIAN_POINT('Ctrl Pts',(-24.3531646875,29.2708333401613,42.1809185638423));
#12503=CARTESIAN_POINT('Ctrl Pts',(-35.6555077526845,29.062500006828,35.6555077526845));
#12504=CARTESIAN_POINT('Ctrl Pts',(-42.1809185638422,28.8541666734946,24.3531646875));
#12505=CARTESIAN_POINT('Ctrl Pts',(-48.706329375,28.6458333401613,13.0508216223155));
#12506=CARTESIAN_POINT('Ctrl Pts',(-48.706329375,28.437500006828,-1.8898197019151E-14));
#12507=CARTESIAN_POINT('Ctrl Pts',(-46.,60.,0.));
#12508=CARTESIAN_POINT('Ctrl Pts',(-46.,59.7916666666667,-12.3256628518316));
#12509=CARTESIAN_POINT('Ctrl Pts',(-39.8371685740842,59.5833333333333,-23.));
#12510=CARTESIAN_POINT('Ctrl Pts',(-33.6743371481684,59.375,-33.6743371481684));
#12511=CARTESIAN_POINT('Ctrl Pts',(-23.,59.1666666666667,-39.8371685740842));
#12512=CARTESIAN_POINT('Ctrl Pts',(-12.3256628518317,58.9583333333333,-46.));
#12513=CARTESIAN_POINT('Ctrl Pts',(-2.81668763803891E-15,58.75,-46.));
#12514=CARTESIAN_POINT('Ctrl Pts',(12.3256628518316,58.5416666666667,-46.));
#12515=CARTESIAN_POINT('Ctrl Pts',(23.,58.3333333333333,-39.8371685740842));
#12516=CARTESIAN_POINT('Ctrl Pts',(33.6743371481683,58.125,-33.6743371481684));
#12517=CARTESIAN_POINT('Ctrl Pts',(39.8371685740842,57.9166666666667,-23.));
#12518=CARTESIAN_POINT('Ctrl Pts',(46.,57.7083333333333,-12.3256628518317));
#12519=CARTESIAN_POINT('Ctrl Pts',(46.,57.5,-5.63337527607782E-15));
#12520=CARTESIAN_POINT('Ctrl Pts',(46.,57.2916666666667,12.3256628518316));
#12521=CARTESIAN_POINT('Ctrl Pts',(39.8371685740842,57.0833333333333,23.));
#12522=CARTESIAN_POINT('Ctrl Pts',(33.6743371481684,56.875,33.6743371481683));
#12523=CARTESIAN_POINT('Ctrl Pts',(23.,56.6666666666667,39.8371685740842));
#12524=CARTESIAN_POINT('Ctrl Pts',(12.3256628518317,56.4583333333333,46.));
#12525=CARTESIAN_POINT('Ctrl Pts',(8.45006291411674E-15,56.25,46.));
#12526=CARTESIAN_POINT('Ctrl Pts',(-12.3256628518316,56.0416666666667,46.));
#12527=CARTESIAN_POINT('Ctrl Pts',(-23.,55.8333333333333,39.8371685740842));
#12528=CARTESIAN_POINT('Ctrl Pts',(-33.6743371481683,55.625,33.6743371481684));
#12529=CARTESIAN_POINT('Ctrl Pts',(-39.8371685740842,55.4166666666667,23.));
#12530=CARTESIAN_POINT('Ctrl Pts',(-46.,55.2083333333333,12.3256628518317));
#12531=CARTESIAN_POINT('Ctrl Pts',(-46.,55.,0.));
#12532=CARTESIAN_POINT('Ctrl Pts',(-46.,54.7916666666667,-12.3256628518316));
#12533=CARTESIAN_POINT('Ctrl Pts',(-39.8371685740842,54.5833333333333,-23.));
#12534=CARTESIAN_POINT('Ctrl Pts',(-33.6743371481684,54.375,-33.6743371481684));
#12535=CARTESIAN_POINT('Ctrl Pts',(-23.,54.1666666666667,-39.8371685740842));
#12536=CARTESIAN_POINT('Ctrl Pts',(-12.3256628518317,53.9583333333333,-46.));
#12537=CARTESIAN_POINT('Ctrl Pts',(-2.81668763803891E-15,53.75,-46.));
#12538=CARTESIAN_POINT('Ctrl Pts',(12.3256628518316,53.5416666666667,-46.));
#12539=CARTESIAN_POINT('Ctrl Pts',(23.,53.3333333333333,-39.8371685740842));
#12540=CARTESIAN_POINT('Ctrl Pts',(33.6743371481683,53.125,-33.6743371481684));
#12541=CARTESIAN_POINT('Ctrl Pts',(39.8371685740842,52.9166666666667,-23.));
#12542=CARTESIAN_POINT('Ctrl Pts',(46.,52.7083333333333,-12.3256628518317));
#12543=CARTESIAN_POINT('Ctrl Pts',(46.,52.5,-5.63337527607782E-15));
#12544=CARTESIAN_POINT('Ctrl Pts',(46.,52.2916666666667,12.3256628518316));
#12545=CARTESIAN_POINT('Ctrl Pts',(39.8371685740842,52.0833333333333,23.));
#12546=CARTESIAN_POINT('Ctrl Pts',(33.6743371481684,51.875,33.6743371481683));
#12547=CARTESIAN_POINT('Ctrl Pts',(23.,51.6666666666667,39.8371685740842));
#12548=CARTESIAN_POINT('Ctrl Pts',(12.3256628518317,51.4583333333333,46.));
#12549=CARTESIAN_POINT('Ctrl Pts',(8.45006291411674E-15,51.25,46.));
#12550=CARTESIAN_POINT('Ctrl Pts',(-12.3256628518316,51.0416666666667,46.));
#12551=CARTESIAN_POINT('Ctrl Pts',(-23.,50.8333333333333,39.8371685740842));
#12552=CARTESIAN_POINT('Ctrl Pts',(-33.6743371481683,50.625,33.6743371481684));
#12553=CARTESIAN_POINT('Ctrl Pts',(-39.8371685740842,50.4166666666667,23.));
#12554=CARTESIAN_POINT('Ctrl Pts',(-46.,50.2083333333333,12.3256628518317));
#12555=CARTESIAN_POINT('Ctrl Pts',(-46.,50.,0.));
#12556=CARTESIAN_POINT('Ctrl Pts',(-46.,49.7916666666667,-12.3256628518316));
#12557=CARTESIAN_POINT('Ctrl Pts',(-39.8371685740842,49.5833333333333,-23.));
#12558=CARTESIAN_POINT('Ctrl Pts',(-33.6743371481684,49.375,-33.6743371481684));
#12559=CARTESIAN_POINT('Ctrl Pts',(-23.,49.1666666666667,-39.8371685740842));
#12560=CARTESIAN_POINT('Ctrl Pts',(-12.3256628518317,48.9583333333333,-46.));
#12561=CARTESIAN_POINT('Ctrl Pts',(-2.81668763803891E-15,48.75,-46.));
#12562=CARTESIAN_POINT('Ctrl Pts',(12.3256628518316,48.5416666666667,-46.));
#12563=CARTESIAN_POINT('Ctrl Pts',(23.,48.3333333333333,-39.8371685740842));
#12564=CARTESIAN_POINT('Ctrl Pts',(33.6743371481683,48.125,-33.6743371481684));
#12565=CARTESIAN_POINT('Ctrl Pts',(39.8371685740842,47.9166666666667,-23.));
#12566=CARTESIAN_POINT('Ctrl Pts',(46.,47.7083333333333,-12.3256628518317));
#12567=CARTESIAN_POINT('Ctrl Pts',(46.,47.5,-5.63337527607782E-15));
#12568=CARTESIAN_POINT('Ctrl Pts',(46.,47.2916666666667,12.3256628518316));
#12569=CARTESIAN_POINT('Ctrl Pts',(39.8371685740842,47.0833333333333,23.));
#12570=CARTESIAN_POINT('Ctrl Pts',(33.6743371481684,46.875,33.6743371481683));
#12571=CARTESIAN_POINT('Ctrl Pts',(23.,46.6666666666667,39.8371685740842));
#12572=CARTESIAN_POINT('Ctrl Pts',(12.3256628518317,46.4583333333333,46.));
#12573=CARTESIAN_POINT('Ctrl Pts',(8.45006291411674E-15,46.25,46.));
#12574=CARTESIAN_POINT('Ctrl Pts',(-12.3256628518316,46.0416666666667,46.));
#12575=CARTESIAN_POINT('Ctrl Pts',(-23.,45.8333333333333,39.8371685740842));
#12576=CARTESIAN_POINT('Ctrl Pts',(-33.6743371481683,45.625,33.6743371481684));
#12577=CARTESIAN_POINT('Ctrl Pts',(-39.8371685740842,45.4166666666667,23.));
#12578=CARTESIAN_POINT('Ctrl Pts',(-46.,45.2083333333333,12.3256628518317));
#12579=CARTESIAN_POINT('Ctrl Pts',(-46.,45.,0.));
#12580=CARTESIAN_POINT('Ctrl Pts',(-46.,44.7916666666667,-12.3256628518316));
#12581=CARTESIAN_POINT('Ctrl Pts',(-39.8371685740842,44.5833333333333,-23.));
#12582=CARTESIAN_POINT('Ctrl Pts',(-33.6743371481684,44.375,-33.6743371481684));
#12583=CARTESIAN_POINT('Ctrl Pts',(-23.,44.1666666666667,-39.8371685740842));
#12584=CARTESIAN_POINT('Ctrl Pts',(-12.3256628518317,43.9583333333333,-46.));
#12585=CARTESIAN_POINT('Ctrl Pts',(-2.81668763803891E-15,43.75,-46.));
#12586=CARTESIAN_POINT('Ctrl Pts',(12.3256628518316,43.5416666666667,-46.));
#12587=CARTESIAN_POINT('Ctrl Pts',(23.,43.3333333333333,-39.8371685740842));
#12588=CARTESIAN_POINT('Ctrl Pts',(33.6743371481683,43.125,-33.6743371481684));
#12589=CARTESIAN_POINT('Ctrl Pts',(39.8371685740842,42.9166666666667,-23.));
#12590=CARTESIAN_POINT('Ctrl Pts',(46.,42.7083333333333,-12.3256628518317));
#12591=CARTESIAN_POINT('Ctrl Pts',(46.,42.5,-5.63337527607782E-15));
#12592=CARTESIAN_POINT('Ctrl Pts',(46.,42.2916666666667,12.3256628518316));
#12593=CARTESIAN_POINT('Ctrl Pts',(39.8371685740842,42.0833333333333,23.));
#12594=CARTESIAN_POINT('Ctrl Pts',(33.6743371481684,41.875,33.6743371481683));
#12595=CARTESIAN_POINT('Ctrl Pts',(23.,41.6666666666667,39.8371685740842));
#12596=CARTESIAN_POINT('Ctrl Pts',(12.3256628518317,41.4583333333333,46.));
#12597=CARTESIAN_POINT('Ctrl Pts',(8.45006291411674E-15,41.25,46.));
#12598=CARTESIAN_POINT('Ctrl Pts',(-12.3256628518316,41.0416666666667,46.));
#12599=CARTESIAN_POINT('Ctrl Pts',(-23.,40.8333333333333,39.8371685740842));
#12600=CARTESIAN_POINT('Ctrl Pts',(-33.6743371481683,40.625,33.6743371481684));
#12601=CARTESIAN_POINT('Ctrl Pts',(-39.8371685740842,40.4166666666667,23.));
#12602=CARTESIAN_POINT('Ctrl Pts',(-46.,40.2083333333333,12.3256628518317));
#12603=CARTESIAN_POINT('Ctrl Pts',(-46.,40.,0.));
#12604=CARTESIAN_POINT('Ctrl Pts',(-46.,39.7916666666667,-12.3256628518316));
#12605=CARTESIAN_POINT('Ctrl Pts',(-39.8371685740842,39.5833333333333,-23.));
#12606=CARTESIAN_POINT('Ctrl Pts',(-33.6743371481684,39.375,-33.6743371481684));
#12607=CARTESIAN_POINT('Ctrl Pts',(-23.,39.1666666666667,-39.8371685740842));
#12608=CARTESIAN_POINT('Ctrl Pts',(-12.3256628518317,38.9583333333333,-46.));
#12609=CARTESIAN_POINT('Ctrl Pts',(-2.81668763803891E-15,38.75,-46.));
#12610=CARTESIAN_POINT('Ctrl Pts',(12.3256628518316,38.5416666666667,-46.));
#12611=CARTESIAN_POINT('Ctrl Pts',(23.,38.3333333333333,-39.8371685740842));
#12612=CARTESIAN_POINT('Ctrl Pts',(33.6743371481683,38.125,-33.6743371481684));
#12613=CARTESIAN_POINT('Ctrl Pts',(39.8371685740842,37.9166666666667,-23.));
#12614=CARTESIAN_POINT('Ctrl Pts',(46.,37.7083333333333,-12.3256628518317));
#12615=CARTESIAN_POINT('Ctrl Pts',(46.,37.5,-5.63337527607782E-15));
#12616=CARTESIAN_POINT('Ctrl Pts',(46.,37.2916666666667,12.3256628518316));
#12617=CARTESIAN_POINT('Ctrl Pts',(39.8371685740842,37.0833333333333,23.));
#12618=CARTESIAN_POINT('Ctrl Pts',(33.6743371481684,36.875,33.6743371481683));
#12619=CARTESIAN_POINT('Ctrl Pts',(23.,36.6666666666667,39.8371685740842));
#12620=CARTESIAN_POINT('Ctrl Pts',(12.3256628518317,36.4583333333333,46.));
#12621=CARTESIAN_POINT('Ctrl Pts',(8.45006291411674E-15,36.25,46.));
#12622=CARTESIAN_POINT('Ctrl Pts',(-12.3256628518316,36.0416666666667,46.));
#12623=CARTESIAN_POINT('Ctrl Pts',(-23.,35.8333333333333,39.8371685740842));
#12624=CARTESIAN_POINT('Ctrl Pts',(-33.6743371481683,35.625,33.6743371481684));
#12625=CARTESIAN_POINT('Ctrl Pts',(-39.8371685740842,35.4166666666667,23.));
#12626=CARTESIAN_POINT('Ctrl Pts',(-46.,35.2083333333333,12.3256628518317));
#12627=CARTESIAN_POINT('Ctrl Pts',(-46.,35.,0.));
#12628=CARTESIAN_POINT('Ctrl Pts',(-46.,34.7916666666667,-12.3256628518316));
#12629=CARTESIAN_POINT('Ctrl Pts',(-39.8371685740842,34.5833333333333,-23.));
#12630=CARTESIAN_POINT('Ctrl Pts',(-33.6743371481684,34.375,-33.6743371481684));
#12631=CARTESIAN_POINT('Ctrl Pts',(-23.,34.1666666666667,-39.8371685740842));
#12632=CARTESIAN_POINT('Ctrl Pts',(-12.3256628518317,33.9583333333333,-46.));
#12633=CARTESIAN_POINT('Ctrl Pts',(-2.81668763803891E-15,33.75,-46.));
#12634=CARTESIAN_POINT('Ctrl Pts',(12.3256628518316,33.5416666666667,-46.));
#12635=CARTESIAN_POINT('Ctrl Pts',(23.,33.3333333333333,-39.8371685740842));
#12636=CARTESIAN_POINT('Ctrl Pts',(33.6743371481683,33.125,-33.6743371481684));
#12637=CARTESIAN_POINT('Ctrl Pts',(39.8371685740842,32.9166666666667,-23.));
#12638=CARTESIAN_POINT('Ctrl Pts',(46.,32.7083333333333,-12.3256628518317));
#12639=CARTESIAN_POINT('Ctrl Pts',(46.,32.5,-5.63337527607782E-15));
#12640=CARTESIAN_POINT('Ctrl Pts',(46.,32.2916666666667,12.3256628518316));
#12641=CARTESIAN_POINT('Ctrl Pts',(39.8371685740842,32.0833333333333,23.));
#12642=CARTESIAN_POINT('Ctrl Pts',(33.6743371481684,31.875,33.6743371481683));
#12643=CARTESIAN_POINT('Ctrl Pts',(23.,31.6666666666667,39.8371685740842));
#12644=CARTESIAN_POINT('Ctrl Pts',(12.3256628518317,31.4583333333333,46.));
#12645=CARTESIAN_POINT('Ctrl Pts',(8.45006291411674E-15,31.25,46.));
#12646=CARTESIAN_POINT('Ctrl Pts',(-12.3256628518316,31.0416666666667,46.));
#12647=CARTESIAN_POINT('Ctrl Pts',(-23.,30.8333333333333,39.8371685740842));
#12648=CARTESIAN_POINT('Ctrl Pts',(-33.6743371481683,30.625,33.6743371481684));
#12649=CARTESIAN_POINT('Ctrl Pts',(-39.8371685740842,30.4166666666667,23.));
#12650=CARTESIAN_POINT('Ctrl Pts',(-46.,30.2083333333333,12.3256628518317));
#12651=CARTESIAN_POINT('Ctrl Pts',(-46.,30.,0.));
#12652=CARTESIAN_POINT('Ctrl Pts',(45.7957082162897,47.5741208584476,-4.33048599679672));
#12653=CARTESIAN_POINT('Ctrl Pts',(46.027322302781,47.4406160752063,-4.33048599679672));
#12654=CARTESIAN_POINT('Ctrl Pts',(46.4905476657728,47.1736016336912,-4.33048599679667));
#12655=CARTESIAN_POINT('Ctrl Pts',(46.9537676533565,46.9065778670208,-4.33048599679672));
#12656=CARTESIAN_POINT('Ctrl Pts',(47.6280672732221,46.5178683162597,-4.33048599679672));
#12657=CARTESIAN_POINT('Ctrl Pts',(48.0707534890442,46.2626647328764,-4.33048599679671));
#12658=CARTESIAN_POINT('Ctrl Pts',(48.5134353784344,46.0074536451604,-4.33048599679671));
#12659=CARTESIAN_POINT('Ctrl Pts',(3.61292728433799,47.1292520480092,-48.5721450795008));
#12660=CARTESIAN_POINT('Ctrl Pts',(3.61292728433799,47.2624339185675,-48.3403451622817));
#12661=CARTESIAN_POINT('Ctrl Pts',(3.612927284338,47.395608829009,-48.1085412459393));
#12662=CARTESIAN_POINT('Ctrl Pts',(3.612927284338,47.6619441142016,-47.6449250631479));
#12663=CARTESIAN_POINT('Ctrl Pts',(3.61292728433804,47.7951044891727,-47.4131127965212));
#12664=CARTESIAN_POINT('Ctrl Pts',(3.61292728433804,47.9282572703914,-47.1812961682826));
#12665=CARTESIAN_POINT('Ctrl Pts',(3.61292728433804,48.1816295626638,-46.7401795055578));
#12666=CARTESIAN_POINT('Ctrl Pts',(3.61292728433796,48.4349743764897,-46.2990470581854));
#12667=CARTESIAN_POINT('Ctrl Pts',(3.61292728433796,48.688289262853,-45.8578974271399));
#12668=CARTESIAN_POINT('Ctrl Pts',(-48.706329375,58.437500006828,-1.8898197019151E-14));
#12669=CARTESIAN_POINT('Ctrl Pts',(-48.706329375,58.2291666734946,-13.0508216223155));
#12670=CARTESIAN_POINT('Ctrl Pts',(-42.1809185638422,58.0208333401613,-24.3531646875));
#12671=CARTESIAN_POINT('Ctrl Pts',(-35.6555077526845,57.812500006828,-35.6555077526845));
#12672=CARTESIAN_POINT('Ctrl Pts',(-24.3531646875,57.6041666734946,-42.1809185638422));
#12673=CARTESIAN_POINT('Ctrl Pts',(-13.0508216223155,57.3958333401613,-48.706329375));
#12674=CARTESIAN_POINT('Ctrl Pts',(1.59157945007855E-14,57.187500006828,
-48.706329375));
#12675=CARTESIAN_POINT('Ctrl Pts',(13.0508216223155,56.9791666734946,-48.706329375));
#12676=CARTESIAN_POINT('Ctrl Pts',(24.3531646875,56.7708333401613,-42.1809185638422));
#12677=CARTESIAN_POINT('Ctrl Pts',(35.6555077526845,56.562500006828,-35.6555077526845));
#12678=CARTESIAN_POINT('Ctrl Pts',(42.1809185638422,56.3541666734946,-24.3531646875));
#12679=CARTESIAN_POINT('Ctrl Pts',(48.706329375,56.1458333401613,-13.0508216223155));
#12680=CARTESIAN_POINT('Ctrl Pts',(48.706329375,55.937500006828,1.293339198242E-14));
#12681=CARTESIAN_POINT('Ctrl Pts',(48.706329375,55.7291666734946,13.0508216223155));
#12682=CARTESIAN_POINT('Ctrl Pts',(42.1809185638422,55.5208333401613,24.3531646875));
#12683=CARTESIAN_POINT('Ctrl Pts',(35.6555077526845,55.312500006828,35.6555077526845));
#12684=CARTESIAN_POINT('Ctrl Pts',(24.3531646875,55.1041666734946,42.1809185638422));
#12685=CARTESIAN_POINT('Ctrl Pts',(13.0508216223155,54.8958333401613,48.706329375));
#12686=CARTESIAN_POINT('Ctrl Pts',(-9.95098946405443E-15,54.687500006828,
48.706329375));
#12687=CARTESIAN_POINT('Ctrl Pts',(-13.0508216223155,54.4791666734946,48.706329375));
#12688=CARTESIAN_POINT('Ctrl Pts',(-24.3531646875,54.2708333401613,42.1809185638423));
#12689=CARTESIAN_POINT('Ctrl Pts',(-35.6555077526845,54.062500006828,35.6555077526845));
#12690=CARTESIAN_POINT('Ctrl Pts',(-42.1809185638422,53.8541666734946,24.3531646875));
#12691=CARTESIAN_POINT('Ctrl Pts',(-48.706329375,53.6458333401613,13.0508216223155));
#12692=CARTESIAN_POINT('Ctrl Pts',(-48.706329375,53.437500006828,-1.8898197019151E-14));
#12693=CARTESIAN_POINT('Ctrl Pts',(-48.706329375,53.2291666734946,-13.0508216223155));
#12694=CARTESIAN_POINT('Ctrl Pts',(-42.1809185638422,53.0208333401613,-24.3531646875));
#12695=CARTESIAN_POINT('Ctrl Pts',(-35.6555077526845,52.812500006828,-35.6555077526845));
#12696=CARTESIAN_POINT('Ctrl Pts',(-24.3531646875,52.6041666734946,-42.1809185638422));
#12697=CARTESIAN_POINT('Ctrl Pts',(-13.0508216223155,52.3958333401613,-48.706329375));
#12698=CARTESIAN_POINT('Ctrl Pts',(1.59157945007855E-14,52.187500006828,
-48.706329375));
#12699=CARTESIAN_POINT('Ctrl Pts',(13.0508216223155,51.9791666734946,-48.706329375));
#12700=CARTESIAN_POINT('Ctrl Pts',(24.3531646875,51.7708333401613,-42.1809185638422));
#12701=CARTESIAN_POINT('Ctrl Pts',(35.6555077526845,51.562500006828,-35.6555077526845));
#12702=CARTESIAN_POINT('Ctrl Pts',(42.1809185638422,51.3541666734946,-24.3531646875));
#12703=CARTESIAN_POINT('Ctrl Pts',(48.706329375,51.1458333401613,-13.0508216223155));
#12704=CARTESIAN_POINT('Ctrl Pts',(48.706329375,50.937500006828,1.293339198242E-14));
#12705=CARTESIAN_POINT('Ctrl Pts',(48.706329375,50.7291666734946,13.0508216223155));
#12706=CARTESIAN_POINT('Ctrl Pts',(42.1809185638422,50.5208333401613,24.3531646875));
#12707=CARTESIAN_POINT('Ctrl Pts',(35.6555077526845,50.312500006828,35.6555077526845));
#12708=CARTESIAN_POINT('Ctrl Pts',(24.3531646875,50.1041666734946,42.1809185638422));
#12709=CARTESIAN_POINT('Ctrl Pts',(13.0508216223155,49.8958333401613,48.706329375));
#12710=CARTESIAN_POINT('Ctrl Pts',(-9.95098946405443E-15,49.687500006828,
48.706329375));
#12711=CARTESIAN_POINT('Ctrl Pts',(-13.0508216223155,49.4791666734946,48.706329375));
#12712=CARTESIAN_POINT('Ctrl Pts',(-24.3531646875,49.2708333401613,42.1809185638423));
#12713=CARTESIAN_POINT('Ctrl Pts',(-35.6555077526845,49.062500006828,35.6555077526845));
#12714=CARTESIAN_POINT('Ctrl Pts',(-42.1809185638422,48.8541666734946,24.3531646875));
#12715=CARTESIAN_POINT('Ctrl Pts',(-48.706329375,48.6458333401613,13.0508216223155));
#12716=CARTESIAN_POINT('Ctrl Pts',(-48.706329375,48.437500006828,-1.8898197019151E-14));
#12717=CARTESIAN_POINT('Ctrl Pts',(-48.706329375,48.2291666734946,-13.0508216223155));
#12718=CARTESIAN_POINT('Ctrl Pts',(-42.1809185638422,48.0208333401613,-24.3531646875));
#12719=CARTESIAN_POINT('Ctrl Pts',(-35.6555077526845,47.812500006828,-35.6555077526845));
#12720=CARTESIAN_POINT('Ctrl Pts',(-24.3531646875,47.6041666734946,-42.1809185638422));
#12721=CARTESIAN_POINT('Ctrl Pts',(-13.0508216223155,47.3958333401613,-48.706329375));
#12722=CARTESIAN_POINT('Ctrl Pts',(1.59157945007855E-14,47.187500006828,
-48.706329375));
#12723=CARTESIAN_POINT('Ctrl Pts',(13.0508216223155,46.9791666734946,-48.706329375));
#12724=CARTESIAN_POINT('Ctrl Pts',(24.3531646875,46.7708333401613,-42.1809185638422));
#12725=CARTESIAN_POINT('Ctrl Pts',(35.6555077526845,46.562500006828,-35.6555077526845));
#12726=CARTESIAN_POINT('Ctrl Pts',(42.1809185638422,46.3541666734946,-24.3531646875));
#12727=CARTESIAN_POINT('Ctrl Pts',(48.706329375,46.1458333401613,-13.0508216223155));
#12728=CARTESIAN_POINT('Ctrl Pts',(48.706329375,45.937500006828,1.293339198242E-14));
#12729=CARTESIAN_POINT('Ctrl Pts',(48.706329375,45.7291666734946,13.0508216223155));
#12730=CARTESIAN_POINT('Ctrl Pts',(42.1809185638422,45.5208333401613,24.3531646875));
#12731=CARTESIAN_POINT('Ctrl Pts',(35.6555077526845,45.312500006828,35.6555077526845));
#12732=CARTESIAN_POINT('Ctrl Pts',(24.3531646875,45.1041666734946,42.1809185638422));
#12733=CARTESIAN_POINT('Ctrl Pts',(13.0508216223155,44.8958333401613,48.706329375));
#12734=CARTESIAN_POINT('Ctrl Pts',(-9.95098946405443E-15,44.687500006828,
48.706329375));
#12735=CARTESIAN_POINT('Ctrl Pts',(-13.0508216223155,44.4791666734946,48.706329375));
#12736=CARTESIAN_POINT('Ctrl Pts',(-24.3531646875,44.2708333401613,42.1809185638423));
#12737=CARTESIAN_POINT('Ctrl Pts',(-35.6555077526845,44.062500006828,35.6555077526845));
#12738=CARTESIAN_POINT('Ctrl Pts',(-42.1809185638422,43.8541666734946,24.3531646875));
#12739=CARTESIAN_POINT('Ctrl Pts',(-48.706329375,43.6458333401613,13.0508216223155));
#12740=CARTESIAN_POINT('Ctrl Pts',(-48.706329375,43.437500006828,-1.8898197019151E-14));
#12741=CARTESIAN_POINT('Ctrl Pts',(-48.706329375,43.2291666734946,-13.0508216223155));
#12742=CARTESIAN_POINT('Ctrl Pts',(-42.1809185638422,43.0208333401613,-24.3531646875));
#12743=CARTESIAN_POINT('Ctrl Pts',(-35.6555077526845,42.812500006828,-35.6555077526845));
#12744=CARTESIAN_POINT('Ctrl Pts',(-24.3531646875,42.6041666734946,-42.1809185638422));
#12745=CARTESIAN_POINT('Ctrl Pts',(-13.0508216223155,42.3958333401613,-48.706329375));
#12746=CARTESIAN_POINT('Ctrl Pts',(1.59157945007855E-14,42.187500006828,
-48.706329375));
#12747=CARTESIAN_POINT('Ctrl Pts',(13.0508216223155,41.9791666734946,-48.706329375));
#12748=CARTESIAN_POINT('Ctrl Pts',(24.3531646875,41.7708333401613,-42.1809185638422));
#12749=CARTESIAN_POINT('Ctrl Pts',(35.6555077526845,41.562500006828,-35.6555077526845));
#12750=CARTESIAN_POINT('Ctrl Pts',(42.1809185638422,41.3541666734946,-24.3531646875));
#12751=CARTESIAN_POINT('Ctrl Pts',(48.706329375,41.1458333401613,-13.0508216223155));
#12752=CARTESIAN_POINT('Ctrl Pts',(48.706329375,40.937500006828,1.293339198242E-14));
#12753=CARTESIAN_POINT('Ctrl Pts',(48.706329375,40.7291666734946,13.0508216223155));
#12754=CARTESIAN_POINT('Ctrl Pts',(42.1809185638422,40.5208333401613,24.3531646875));
#12755=CARTESIAN_POINT('Ctrl Pts',(35.6555077526845,40.312500006828,35.6555077526845));
#12756=CARTESIAN_POINT('Ctrl Pts',(24.3531646875,40.1041666734946,42.1809185638422));
#12757=CARTESIAN_POINT('Ctrl Pts',(13.0508216223155,39.8958333401613,48.706329375));
#12758=CARTESIAN_POINT('Ctrl Pts',(-9.95098946405443E-15,39.687500006828,
48.706329375));
#12759=CARTESIAN_POINT('Ctrl Pts',(-13.0508216223155,39.4791666734946,48.706329375));
#12760=CARTESIAN_POINT('Ctrl Pts',(-24.3531646875,39.2708333401613,42.1809185638423));
#12761=CARTESIAN_POINT('Ctrl Pts',(-35.6555077526845,39.062500006828,35.6555077526845));
#12762=CARTESIAN_POINT('Ctrl Pts',(-42.1809185638422,38.8541666734946,24.3531646875));
#12763=CARTESIAN_POINT('Ctrl Pts',(-48.706329375,38.6458333401613,13.0508216223155));
#12764=CARTESIAN_POINT('Ctrl Pts',(-48.706329375,38.437500006828,-1.8898197019151E-14));
#12765=CARTESIAN_POINT('Ctrl Pts',(-48.706329375,38.2291666734946,-13.0508216223155));
#12766=CARTESIAN_POINT('Ctrl Pts',(-42.1809185638422,38.0208333401613,-24.3531646875));
#12767=CARTESIAN_POINT('Ctrl Pts',(-35.6555077526845,37.812500006828,-35.6555077526845));
#12768=CARTESIAN_POINT('Ctrl Pts',(-24.3531646875,37.6041666734946,-42.1809185638422));
#12769=CARTESIAN_POINT('Ctrl Pts',(-13.0508216223155,37.3958333401613,-48.706329375));
#12770=CARTESIAN_POINT('Ctrl Pts',(1.59157945007855E-14,37.187500006828,
-48.706329375));
#12771=CARTESIAN_POINT('Ctrl Pts',(13.0508216223155,36.9791666734946,-48.706329375));
#12772=CARTESIAN_POINT('Ctrl Pts',(24.3531646875,36.7708333401613,-42.1809185638422));
#12773=CARTESIAN_POINT('Ctrl Pts',(35.6555077526845,36.562500006828,-35.6555077526845));
#12774=CARTESIAN_POINT('Ctrl Pts',(42.1809185638422,36.3541666734946,-24.3531646875));
#12775=CARTESIAN_POINT('Ctrl Pts',(48.706329375,36.1458333401613,-13.0508216223155));
#12776=CARTESIAN_POINT('Ctrl Pts',(48.706329375,35.937500006828,1.293339198242E-14));
#12777=CARTESIAN_POINT('Ctrl Pts',(48.706329375,35.7291666734946,13.0508216223155));
#12778=CARTESIAN_POINT('Ctrl Pts',(42.1809185638422,35.5208333401613,24.3531646875));
#12779=CARTESIAN_POINT('Ctrl Pts',(35.6555077526845,35.312500006828,35.6555077526845));
#12780=CARTESIAN_POINT('Ctrl Pts',(24.3531646875,35.1041666734946,42.1809185638422));
#12781=CARTESIAN_POINT('Ctrl Pts',(13.0508216223155,34.8958333401613,48.706329375));
#12782=CARTESIAN_POINT('Ctrl Pts',(-9.95098946405443E-15,34.687500006828,
48.706329375));
#12783=CARTESIAN_POINT('Ctrl Pts',(-13.0508216223155,34.4791666734946,48.706329375));
#12784=CARTESIAN_POINT('Ctrl Pts',(-24.3531646875,34.2708333401613,42.1809185638423));
#12785=CARTESIAN_POINT('Ctrl Pts',(-35.6555077526845,34.062500006828,35.6555077526845));
#12786=CARTESIAN_POINT('Ctrl Pts',(-42.1809185638422,33.8541666734946,24.3531646875));
#12787=CARTESIAN_POINT('Ctrl Pts',(-48.706329375,33.6458333401613,13.0508216223155));
#12788=CARTESIAN_POINT('Ctrl Pts',(-48.706329375,33.437500006828,-1.8898197019151E-14));
#12789=CARTESIAN_POINT('Ctrl Pts',(-48.706329375,33.2291666734946,-13.0508216223155));
#12790=CARTESIAN_POINT('Ctrl Pts',(-42.1809185638422,33.0208333401613,-24.3531646875));
#12791=CARTESIAN_POINT('Ctrl Pts',(-35.6555077526845,32.812500006828,-35.6555077526845));
#12792=CARTESIAN_POINT('Ctrl Pts',(-24.3531646875,32.6041666734946,-42.1809185638422));
#12793=CARTESIAN_POINT('Ctrl Pts',(-13.0508216223155,32.3958333401613,-48.706329375));
#12794=CARTESIAN_POINT('Ctrl Pts',(1.59157945007855E-14,32.187500006828,
-48.706329375));
#12795=CARTESIAN_POINT('Ctrl Pts',(13.0508216223155,31.9791666734946,-48.706329375));
#12796=CARTESIAN_POINT('Ctrl Pts',(24.3531646875,31.7708333401613,-42.1809185638422));
#12797=CARTESIAN_POINT('Ctrl Pts',(35.6555077526845,31.562500006828,-35.6555077526845));
#12798=CARTESIAN_POINT('Ctrl Pts',(42.1809185638422,31.3541666734946,-24.3531646875));
#12799=CARTESIAN_POINT('Ctrl Pts',(48.706329375,31.1458333401613,-13.0508216223155));
#12800=CARTESIAN_POINT('Ctrl Pts',(48.706329375,30.937500006828,1.293339198242E-14));
#12801=CARTESIAN_POINT('Ctrl Pts',(48.706329375,30.7291666734946,13.0508216223155));
#12802=CARTESIAN_POINT('Ctrl Pts',(42.1809185638422,30.5208333401613,24.3531646875));
#12803=CARTESIAN_POINT('Ctrl Pts',(35.6555077526845,30.312500006828,35.6555077526845));
#12804=CARTESIAN_POINT('Ctrl Pts',(24.3531646875,30.1041666734946,42.1809185638422));
#12805=CARTESIAN_POINT('Ctrl Pts',(13.0508216223155,29.8958333401613,48.706329375));
#12806=CARTESIAN_POINT('Ctrl Pts',(-9.95098946405443E-15,29.687500006828,
48.706329375));
#12807=CARTESIAN_POINT('Ctrl Pts',(-13.0508216223155,29.4791666734946,48.706329375));
#12808=CARTESIAN_POINT('Ctrl Pts',(-24.3531646875,29.2708333401613,42.1809185638423));
#12809=CARTESIAN_POINT('Ctrl Pts',(-35.6555077526845,29.062500006828,35.6555077526845));
#12810=CARTESIAN_POINT('Ctrl Pts',(-42.1809185638422,28.8541666734946,24.3531646875));
#12811=CARTESIAN_POINT('Ctrl Pts',(-48.706329375,28.6458333401613,13.0508216223155));
#12812=CARTESIAN_POINT('Ctrl Pts',(-48.706329375,28.437500006828,-1.8898197019151E-14));
#12813=CARTESIAN_POINT('Ctrl Pts',(-46.,60.,0.));
#12814=CARTESIAN_POINT('Ctrl Pts',(-46.,59.7916666666667,-12.3256628518316));
#12815=CARTESIAN_POINT('Ctrl Pts',(-39.8371685740842,59.5833333333333,-23.));
#12816=CARTESIAN_POINT('Ctrl Pts',(-33.6743371481684,59.375,-33.6743371481684));
#12817=CARTESIAN_POINT('Ctrl Pts',(-23.,59.1666666666667,-39.8371685740842));
#12818=CARTESIAN_POINT('Ctrl Pts',(-12.3256628518317,58.9583333333333,-46.));
#12819=CARTESIAN_POINT('Ctrl Pts',(-2.81668763803891E-15,58.75,-46.));
#12820=CARTESIAN_POINT('Ctrl Pts',(12.3256628518316,58.5416666666667,-46.));
#12821=CARTESIAN_POINT('Ctrl Pts',(23.,58.3333333333333,-39.8371685740842));
#12822=CARTESIAN_POINT('Ctrl Pts',(33.6743371481683,58.125,-33.6743371481684));
#12823=CARTESIAN_POINT('Ctrl Pts',(39.8371685740842,57.9166666666667,-23.));
#12824=CARTESIAN_POINT('Ctrl Pts',(46.,57.7083333333333,-12.3256628518317));
#12825=CARTESIAN_POINT('Ctrl Pts',(46.,57.5,-5.63337527607782E-15));
#12826=CARTESIAN_POINT('Ctrl Pts',(46.,57.2916666666667,12.3256628518316));
#12827=CARTESIAN_POINT('Ctrl Pts',(39.8371685740842,57.0833333333333,23.));
#12828=CARTESIAN_POINT('Ctrl Pts',(33.6743371481684,56.875,33.6743371481683));
#12829=CARTESIAN_POINT('Ctrl Pts',(23.,56.6666666666667,39.8371685740842));
#12830=CARTESIAN_POINT('Ctrl Pts',(12.3256628518317,56.4583333333333,46.));
#12831=CARTESIAN_POINT('Ctrl Pts',(8.45006291411674E-15,56.25,46.));
#12832=CARTESIAN_POINT('Ctrl Pts',(-12.3256628518316,56.0416666666667,46.));
#12833=CARTESIAN_POINT('Ctrl Pts',(-23.,55.8333333333333,39.8371685740842));
#12834=CARTESIAN_POINT('Ctrl Pts',(-33.6743371481683,55.625,33.6743371481684));
#12835=CARTESIAN_POINT('Ctrl Pts',(-39.8371685740842,55.4166666666667,23.));
#12836=CARTESIAN_POINT('Ctrl Pts',(-46.,55.2083333333333,12.3256628518317));
#12837=CARTESIAN_POINT('Ctrl Pts',(-46.,55.,0.));
#12838=CARTESIAN_POINT('Ctrl Pts',(-46.,54.7916666666667,-12.3256628518316));
#12839=CARTESIAN_POINT('Ctrl Pts',(-39.8371685740842,54.5833333333333,-23.));
#12840=CARTESIAN_POINT('Ctrl Pts',(-33.6743371481684,54.375,-33.6743371481684));
#12841=CARTESIAN_POINT('Ctrl Pts',(-23.,54.1666666666667,-39.8371685740842));
#12842=CARTESIAN_POINT('Ctrl Pts',(-12.3256628518317,53.9583333333333,-46.));
#12843=CARTESIAN_POINT('Ctrl Pts',(-2.81668763803891E-15,53.75,-46.));
#12844=CARTESIAN_POINT('Ctrl Pts',(12.3256628518316,53.5416666666667,-46.));
#12845=CARTESIAN_POINT('Ctrl Pts',(23.,53.3333333333333,-39.8371685740842));
#12846=CARTESIAN_POINT('Ctrl Pts',(33.6743371481683,53.125,-33.6743371481684));
#12847=CARTESIAN_POINT('Ctrl Pts',(39.8371685740842,52.9166666666667,-23.));
#12848=CARTESIAN_POINT('Ctrl Pts',(46.,52.7083333333333,-12.3256628518317));
#12849=CARTESIAN_POINT('Ctrl Pts',(46.,52.5,-5.63337527607782E-15));
#12850=CARTESIAN_POINT('Ctrl Pts',(46.,52.2916666666667,12.3256628518316));
#12851=CARTESIAN_POINT('Ctrl Pts',(39.8371685740842,52.0833333333333,23.));
#12852=CARTESIAN_POINT('Ctrl Pts',(33.6743371481684,51.875,33.6743371481683));
#12853=CARTESIAN_POINT('Ctrl Pts',(23.,51.6666666666667,39.8371685740842));
#12854=CARTESIAN_POINT('Ctrl Pts',(12.3256628518317,51.4583333333333,46.));
#12855=CARTESIAN_POINT('Ctrl Pts',(8.45006291411674E-15,51.25,46.));
#12856=CARTESIAN_POINT('Ctrl Pts',(-12.3256628518316,51.0416666666667,46.));
#12857=CARTESIAN_POINT('Ctrl Pts',(-23.,50.8333333333333,39.8371685740842));
#12858=CARTESIAN_POINT('Ctrl Pts',(-33.6743371481683,50.625,33.6743371481684));
#12859=CARTESIAN_POINT('Ctrl Pts',(-39.8371685740842,50.4166666666667,23.));
#12860=CARTESIAN_POINT('Ctrl Pts',(-46.,50.2083333333333,12.3256628518317));
#12861=CARTESIAN_POINT('Ctrl Pts',(-46.,50.,0.));
#12862=CARTESIAN_POINT('Ctrl Pts',(-46.,49.7916666666667,-12.3256628518316));
#12863=CARTESIAN_POINT('Ctrl Pts',(-39.8371685740842,49.5833333333333,-23.));
#12864=CARTESIAN_POINT('Ctrl Pts',(-33.6743371481684,49.375,-33.6743371481684));
#12865=CARTESIAN_POINT('Ctrl Pts',(-23.,49.1666666666667,-39.8371685740842));
#12866=CARTESIAN_POINT('Ctrl Pts',(-12.3256628518317,48.9583333333333,-46.));
#12867=CARTESIAN_POINT('Ctrl Pts',(-2.81668763803891E-15,48.75,-46.));
#12868=CARTESIAN_POINT('Ctrl Pts',(12.3256628518316,48.5416666666667,-46.));
#12869=CARTESIAN_POINT('Ctrl Pts',(23.,48.3333333333333,-39.8371685740842));
#12870=CARTESIAN_POINT('Ctrl Pts',(33.6743371481683,48.125,-33.6743371481684));
#12871=CARTESIAN_POINT('Ctrl Pts',(39.8371685740842,47.9166666666667,-23.));
#12872=CARTESIAN_POINT('Ctrl Pts',(46.,47.7083333333333,-12.3256628518317));
#12873=CARTESIAN_POINT('Ctrl Pts',(46.,47.5,-5.63337527607782E-15));
#12874=CARTESIAN_POINT('Ctrl Pts',(46.,47.2916666666667,12.3256628518316));
#12875=CARTESIAN_POINT('Ctrl Pts',(39.8371685740842,47.0833333333333,23.));
#12876=CARTESIAN_POINT('Ctrl Pts',(33.6743371481684,46.875,33.6743371481683));
#12877=CARTESIAN_POINT('Ctrl Pts',(23.,46.6666666666667,39.8371685740842));
#12878=CARTESIAN_POINT('Ctrl Pts',(12.3256628518317,46.4583333333333,46.));
#12879=CARTESIAN_POINT('Ctrl Pts',(8.45006291411674E-15,46.25,46.));
#12880=CARTESIAN_POINT('Ctrl Pts',(-12.3256628518316,46.0416666666667,46.));
#12881=CARTESIAN_POINT('Ctrl Pts',(-23.,45.8333333333333,39.8371685740842));
#12882=CARTESIAN_POINT('Ctrl Pts',(-33.6743371481683,45.625,33.6743371481684));
#12883=CARTESIAN_POINT('Ctrl Pts',(-39.8371685740842,45.4166666666667,23.));
#12884=CARTESIAN_POINT('Ctrl Pts',(-46.,45.2083333333333,12.3256628518317));
#12885=CARTESIAN_POINT('Ctrl Pts',(-46.,45.,0.));
#12886=CARTESIAN_POINT('Ctrl Pts',(-46.,44.7916666666667,-12.3256628518316));
#12887=CARTESIAN_POINT('Ctrl Pts',(-39.8371685740842,44.5833333333333,-23.));
#12888=CARTESIAN_POINT('Ctrl Pts',(-33.6743371481684,44.375,-33.6743371481684));
#12889=CARTESIAN_POINT('Ctrl Pts',(-23.,44.1666666666667,-39.8371685740842));
#12890=CARTESIAN_POINT('Ctrl Pts',(-12.3256628518317,43.9583333333333,-46.));
#12891=CARTESIAN_POINT('Ctrl Pts',(-2.81668763803891E-15,43.75,-46.));
#12892=CARTESIAN_POINT('Ctrl Pts',(12.3256628518316,43.5416666666667,-46.));
#12893=CARTESIAN_POINT('Ctrl Pts',(23.,43.3333333333333,-39.8371685740842));
#12894=CARTESIAN_POINT('Ctrl Pts',(33.6743371481683,43.125,-33.6743371481684));
#12895=CARTESIAN_POINT('Ctrl Pts',(39.8371685740842,42.9166666666667,-23.));
#12896=CARTESIAN_POINT('Ctrl Pts',(46.,42.7083333333333,-12.3256628518317));
#12897=CARTESIAN_POINT('Ctrl Pts',(46.,42.5,-5.63337527607782E-15));
#12898=CARTESIAN_POINT('Ctrl Pts',(46.,42.2916666666667,12.3256628518316));
#12899=CARTESIAN_POINT('Ctrl Pts',(39.8371685740842,42.0833333333333,23.));
#12900=CARTESIAN_POINT('Ctrl Pts',(33.6743371481684,41.875,33.6743371481683));
#12901=CARTESIAN_POINT('Ctrl Pts',(23.,41.6666666666667,39.8371685740842));
#12902=CARTESIAN_POINT('Ctrl Pts',(12.3256628518317,41.4583333333333,46.));
#12903=CARTESIAN_POINT('Ctrl Pts',(8.45006291411674E-15,41.25,46.));
#12904=CARTESIAN_POINT('Ctrl Pts',(-12.3256628518316,41.0416666666667,46.));
#12905=CARTESIAN_POINT('Ctrl Pts',(-23.,40.8333333333333,39.8371685740842));
#12906=CARTESIAN_POINT('Ctrl Pts',(-33.6743371481683,40.625,33.6743371481684));
#12907=CARTESIAN_POINT('Ctrl Pts',(-39.8371685740842,40.4166666666667,23.));
#12908=CARTESIAN_POINT('Ctrl Pts',(-46.,40.2083333333333,12.3256628518317));
#12909=CARTESIAN_POINT('Ctrl Pts',(-46.,40.,0.));
#12910=CARTESIAN_POINT('Ctrl Pts',(-46.,39.7916666666667,-12.3256628518316));
#12911=CARTESIAN_POINT('Ctrl Pts',(-39.8371685740842,39.5833333333333,-23.));
#12912=CARTESIAN_POINT('Ctrl Pts',(-33.6743371481684,39.375,-33.6743371481684));
#12913=CARTESIAN_POINT('Ctrl Pts',(-23.,39.1666666666667,-39.8371685740842));
#12914=CARTESIAN_POINT('Ctrl Pts',(-12.3256628518317,38.9583333333333,-46.));
#12915=CARTESIAN_POINT('Ctrl Pts',(-2.81668763803891E-15,38.75,-46.));
#12916=CARTESIAN_POINT('Ctrl Pts',(12.3256628518316,38.5416666666667,-46.));
#12917=CARTESIAN_POINT('Ctrl Pts',(23.,38.3333333333333,-39.8371685740842));
#12918=CARTESIAN_POINT('Ctrl Pts',(33.6743371481683,38.125,-33.6743371481684));
#12919=CARTESIAN_POINT('Ctrl Pts',(39.8371685740842,37.9166666666667,-23.));
#12920=CARTESIAN_POINT('Ctrl Pts',(46.,37.7083333333333,-12.3256628518317));
#12921=CARTESIAN_POINT('Ctrl Pts',(46.,37.5,-5.63337527607782E-15));
#12922=CARTESIAN_POINT('Ctrl Pts',(46.,37.2916666666667,12.3256628518316));
#12923=CARTESIAN_POINT('Ctrl Pts',(39.8371685740842,37.0833333333333,23.));
#12924=CARTESIAN_POINT('Ctrl Pts',(33.6743371481684,36.875,33.6743371481683));
#12925=CARTESIAN_POINT('Ctrl Pts',(23.,36.6666666666667,39.8371685740842));
#12926=CARTESIAN_POINT('Ctrl Pts',(12.3256628518317,36.4583333333333,46.));
#12927=CARTESIAN_POINT('Ctrl Pts',(8.45006291411674E-15,36.25,46.));
#12928=CARTESIAN_POINT('Ctrl Pts',(-12.3256628518316,36.0416666666667,46.));
#12929=CARTESIAN_POINT('Ctrl Pts',(-23.,35.8333333333333,39.8371685740842));
#12930=CARTESIAN_POINT('Ctrl Pts',(-33.6743371481683,35.625,33.6743371481684));
#12931=CARTESIAN_POINT('Ctrl Pts',(-39.8371685740842,35.4166666666667,23.));
#12932=CARTESIAN_POINT('Ctrl Pts',(-46.,35.2083333333333,12.3256628518317));
#12933=CARTESIAN_POINT('Ctrl Pts',(-46.,35.,0.));
#12934=CARTESIAN_POINT('Ctrl Pts',(-46.,34.7916666666667,-12.3256628518316));
#12935=CARTESIAN_POINT('Ctrl Pts',(-39.8371685740842,34.5833333333333,-23.));
#12936=CARTESIAN_POINT('Ctrl Pts',(-33.6743371481684,34.375,-33.6743371481684));
#12937=CARTESIAN_POINT('Ctrl Pts',(-23.,34.1666666666667,-39.8371685740842));
#12938=CARTESIAN_POINT('Ctrl Pts',(-12.3256628518317,33.9583333333333,-46.));
#12939=CARTESIAN_POINT('Ctrl Pts',(-2.81668763803891E-15,33.75,-46.));
#12940=CARTESIAN_POINT('Ctrl Pts',(12.3256628518316,33.5416666666667,-46.));
#12941=CARTESIAN_POINT('Ctrl Pts',(23.,33.3333333333333,-39.8371685740842));
#12942=CARTESIAN_POINT('Ctrl Pts',(33.6743371481683,33.125,-33.6743371481684));
#12943=CARTESIAN_POINT('Ctrl Pts',(39.8371685740842,32.9166666666667,-23.));
#12944=CARTESIAN_POINT('Ctrl Pts',(46.,32.7083333333333,-12.3256628518317));
#12945=CARTESIAN_POINT('Ctrl Pts',(46.,32.5,-5.63337527607782E-15));
#12946=CARTESIAN_POINT('Ctrl Pts',(46.,32.2916666666667,12.3256628518316));
#12947=CARTESIAN_POINT('Ctrl Pts',(39.8371685740842,32.0833333333333,23.));
#12948=CARTESIAN_POINT('Ctrl Pts',(33.6743371481684,31.875,33.6743371481683));
#12949=CARTESIAN_POINT('Ctrl Pts',(23.,31.6666666666667,39.8371685740842));
#12950=CARTESIAN_POINT('Ctrl Pts',(12.3256628518317,31.4583333333333,46.));
#12951=CARTESIAN_POINT('Ctrl Pts',(8.45006291411674E-15,31.25,46.));
#12952=CARTESIAN_POINT('Ctrl Pts',(-12.3256628518316,31.0416666666667,46.));
#12953=CARTESIAN_POINT('Ctrl Pts',(-23.,30.8333333333333,39.8371685740842));
#12954=CARTESIAN_POINT('Ctrl Pts',(-33.6743371481683,30.625,33.6743371481684));
#12955=CARTESIAN_POINT('Ctrl Pts',(-39.8371685740842,30.4166666666667,23.));
#12956=CARTESIAN_POINT('Ctrl Pts',(-46.,30.2083333333333,12.3256628518317));
#12957=CARTESIAN_POINT('Ctrl Pts',(-46.,30.,0.));
#12958=CARTESIAN_POINT('Ctrl Pts',(48.5725845633798,45.8793483229262,3.60701400320328));
#12959=CARTESIAN_POINT('Ctrl Pts',(48.3407853679392,46.0125314497137,3.60701400320328));
#12960=CARTESIAN_POINT('Ctrl Pts',(48.1089821836664,46.1457076343819,3.60701400320327));
#12961=CARTESIAN_POINT('Ctrl Pts',(47.6453674864979,46.4120455056142,3.60701400320327));
#12962=CARTESIAN_POINT('Ctrl Pts',(47.4135559734254,46.5452071923974,3.60701400320325));
#12963=CARTESIAN_POINT('Ctrl Pts',(47.1817401099609,46.6783613050641,3.60701400320325));
#12964=CARTESIAN_POINT('Ctrl Pts',(46.7406305897488,46.9317328641751,3.60701400320325));
#12965=CARTESIAN_POINT('Ctrl Pts',(46.2995053259033,47.1850770165971,3.60701400320324));
#12966=CARTESIAN_POINT('Ctrl Pts',(45.858362923034,47.438391319744,3.60701400320324));
#12967=CARTESIAN_POINT('Ctrl Pts',(3.61292728433799,46.311710737147,45.8578974271399));
#12968=CARTESIAN_POINT('Ctrl Pts',(3.61292728433798,46.178117727701,46.089460636719));
#12969=CARTESIAN_POINT('Ctrl Pts',(3.61292728433804,45.9109294856547,46.5525857733052));
#12970=CARTESIAN_POINT('Ctrl Pts',(3.61292728433797,45.6437369897944,47.0157084557285));
#12971=CARTESIAN_POINT('Ctrl Pts',(3.61292728433797,45.2553460757965,47.6888965792834));
#12972=CARTESIAN_POINT('Ctrl Pts',(3.61292728433797,45.0005487265709,48.1305218136162));
#12973=CARTESIAN_POINT('Ctrl Pts',(3.61292728433797,44.7457479656467,48.5721450795008));
#12974=CARTESIAN_POINT('Ctrl Pts',(-48.706329375,58.437500006828,-1.8898197019151E-14));
#12975=CARTESIAN_POINT('Ctrl Pts',(-48.706329375,58.2291666734946,-13.0508216223155));
#12976=CARTESIAN_POINT('Ctrl Pts',(-42.1809185638422,58.0208333401613,-24.3531646875));
#12977=CARTESIAN_POINT('Ctrl Pts',(-35.6555077526845,57.812500006828,-35.6555077526845));
#12978=CARTESIAN_POINT('Ctrl Pts',(-24.3531646875,57.6041666734946,-42.1809185638422));
#12979=CARTESIAN_POINT('Ctrl Pts',(-13.0508216223155,57.3958333401613,-48.706329375));
#12980=CARTESIAN_POINT('Ctrl Pts',(1.59157945007855E-14,57.187500006828,
-48.706329375));
#12981=CARTESIAN_POINT('Ctrl Pts',(13.0508216223155,56.9791666734946,-48.706329375));
#12982=CARTESIAN_POINT('Ctrl Pts',(24.3531646875,56.7708333401613,-42.1809185638422));
#12983=CARTESIAN_POINT('Ctrl Pts',(35.6555077526845,56.562500006828,-35.6555077526845));
#12984=CARTESIAN_POINT('Ctrl Pts',(42.1809185638422,56.3541666734946,-24.3531646875));
#12985=CARTESIAN_POINT('Ctrl Pts',(48.706329375,56.1458333401613,-13.0508216223155));
#12986=CARTESIAN_POINT('Ctrl Pts',(48.706329375,55.937500006828,1.293339198242E-14));
#12987=CARTESIAN_POINT('Ctrl Pts',(48.706329375,55.7291666734946,13.0508216223155));
#12988=CARTESIAN_POINT('Ctrl Pts',(42.1809185638422,55.5208333401613,24.3531646875));
#12989=CARTESIAN_POINT('Ctrl Pts',(35.6555077526845,55.312500006828,35.6555077526845));
#12990=CARTESIAN_POINT('Ctrl Pts',(24.3531646875,55.1041666734946,42.1809185638422));
#12991=CARTESIAN_POINT('Ctrl Pts',(13.0508216223155,54.8958333401613,48.706329375));
#12992=CARTESIAN_POINT('Ctrl Pts',(-9.95098946405443E-15,54.687500006828,
48.706329375));
#12993=CARTESIAN_POINT('Ctrl Pts',(-13.0508216223155,54.4791666734946,48.706329375));
#12994=CARTESIAN_POINT('Ctrl Pts',(-24.3531646875,54.2708333401613,42.1809185638423));
#12995=CARTESIAN_POINT('Ctrl Pts',(-35.6555077526845,54.062500006828,35.6555077526845));
#12996=CARTESIAN_POINT('Ctrl Pts',(-42.1809185638422,53.8541666734946,24.3531646875));
#12997=CARTESIAN_POINT('Ctrl Pts',(-48.706329375,53.6458333401613,13.0508216223155));
#12998=CARTESIAN_POINT('Ctrl Pts',(-48.706329375,53.437500006828,-1.8898197019151E-14));
#12999=CARTESIAN_POINT('Ctrl Pts',(-48.706329375,53.2291666734946,-13.0508216223155));
#13000=CARTESIAN_POINT('Ctrl Pts',(-42.1809185638422,53.0208333401613,-24.3531646875));
#13001=CARTESIAN_POINT('Ctrl Pts',(-35.6555077526845,52.812500006828,-35.6555077526845));
#13002=CARTESIAN_POINT('Ctrl Pts',(-24.3531646875,52.6041666734946,-42.1809185638422));
#13003=CARTESIAN_POINT('Ctrl Pts',(-13.0508216223155,52.3958333401613,-48.706329375));
#13004=CARTESIAN_POINT('Ctrl Pts',(1.59157945007855E-14,52.187500006828,
-48.706329375));
#13005=CARTESIAN_POINT('Ctrl Pts',(13.0508216223155,51.9791666734946,-48.706329375));
#13006=CARTESIAN_POINT('Ctrl Pts',(24.3531646875,51.7708333401613,-42.1809185638422));
#13007=CARTESIAN_POINT('Ctrl Pts',(35.6555077526845,51.562500006828,-35.6555077526845));
#13008=CARTESIAN_POINT('Ctrl Pts',(42.1809185638422,51.3541666734946,-24.3531646875));
#13009=CARTESIAN_POINT('Ctrl Pts',(48.706329375,51.1458333401613,-13.0508216223155));
#13010=CARTESIAN_POINT('Ctrl Pts',(48.706329375,50.937500006828,1.293339198242E-14));
#13011=CARTESIAN_POINT('Ctrl Pts',(48.706329375,50.7291666734946,13.0508216223155));
#13012=CARTESIAN_POINT('Ctrl Pts',(42.1809185638422,50.5208333401613,24.3531646875));
#13013=CARTESIAN_POINT('Ctrl Pts',(35.6555077526845,50.312500006828,35.6555077526845));
#13014=CARTESIAN_POINT('Ctrl Pts',(24.3531646875,50.1041666734946,42.1809185638422));
#13015=CARTESIAN_POINT('Ctrl Pts',(13.0508216223155,49.8958333401613,48.706329375));
#13016=CARTESIAN_POINT('Ctrl Pts',(-9.95098946405443E-15,49.687500006828,
48.706329375));
#13017=CARTESIAN_POINT('Ctrl Pts',(-13.0508216223155,49.4791666734946,48.706329375));
#13018=CARTESIAN_POINT('Ctrl Pts',(-24.3531646875,49.2708333401613,42.1809185638423));
#13019=CARTESIAN_POINT('Ctrl Pts',(-35.6555077526845,49.062500006828,35.6555077526845));
#13020=CARTESIAN_POINT('Ctrl Pts',(-42.1809185638422,48.8541666734946,24.3531646875));
#13021=CARTESIAN_POINT('Ctrl Pts',(-48.706329375,48.6458333401613,13.0508216223155));
#13022=CARTESIAN_POINT('Ctrl Pts',(-48.706329375,48.437500006828,-1.8898197019151E-14));
#13023=CARTESIAN_POINT('Ctrl Pts',(-48.706329375,48.2291666734946,-13.0508216223155));
#13024=CARTESIAN_POINT('Ctrl Pts',(-42.1809185638422,48.0208333401613,-24.3531646875));
#13025=CARTESIAN_POINT('Ctrl Pts',(-35.6555077526845,47.812500006828,-35.6555077526845));
#13026=CARTESIAN_POINT('Ctrl Pts',(-24.3531646875,47.6041666734946,-42.1809185638422));
#13027=CARTESIAN_POINT('Ctrl Pts',(-13.0508216223155,47.3958333401613,-48.706329375));
#13028=CARTESIAN_POINT('Ctrl Pts',(1.59157945007855E-14,47.187500006828,
-48.706329375));
#13029=CARTESIAN_POINT('Ctrl Pts',(13.0508216223155,46.9791666734946,-48.706329375));
#13030=CARTESIAN_POINT('Ctrl Pts',(24.3531646875,46.7708333401613,-42.1809185638422));
#13031=CARTESIAN_POINT('Ctrl Pts',(35.6555077526845,46.562500006828,-35.6555077526845));
#13032=CARTESIAN_POINT('Ctrl Pts',(42.1809185638422,46.3541666734946,-24.3531646875));
#13033=CARTESIAN_POINT('Ctrl Pts',(48.706329375,46.1458333401613,-13.0508216223155));
#13034=CARTESIAN_POINT('Ctrl Pts',(48.706329375,45.937500006828,1.293339198242E-14));
#13035=CARTESIAN_POINT('Ctrl Pts',(48.706329375,45.7291666734946,13.0508216223155));
#13036=CARTESIAN_POINT('Ctrl Pts',(42.1809185638422,45.5208333401613,24.3531646875));
#13037=CARTESIAN_POINT('Ctrl Pts',(35.6555077526845,45.312500006828,35.6555077526845));
#13038=CARTESIAN_POINT('Ctrl Pts',(24.3531646875,45.1041666734946,42.1809185638422));
#13039=CARTESIAN_POINT('Ctrl Pts',(13.0508216223155,44.8958333401613,48.706329375));
#13040=CARTESIAN_POINT('Ctrl Pts',(-9.95098946405443E-15,44.687500006828,
48.706329375));
#13041=CARTESIAN_POINT('Ctrl Pts',(-13.0508216223155,44.4791666734946,48.706329375));
#13042=CARTESIAN_POINT('Ctrl Pts',(-24.3531646875,44.2708333401613,42.1809185638423));
#13043=CARTESIAN_POINT('Ctrl Pts',(-35.6555077526845,44.062500006828,35.6555077526845));
#13044=CARTESIAN_POINT('Ctrl Pts',(-42.1809185638422,43.8541666734946,24.3531646875));
#13045=CARTESIAN_POINT('Ctrl Pts',(-48.706329375,43.6458333401613,13.0508216223155));
#13046=CARTESIAN_POINT('Ctrl Pts',(-48.706329375,43.437500006828,-1.8898197019151E-14));
#13047=CARTESIAN_POINT('Ctrl Pts',(-48.706329375,43.2291666734946,-13.0508216223155));
#13048=CARTESIAN_POINT('Ctrl Pts',(-42.1809185638422,43.0208333401613,-24.3531646875));
#13049=CARTESIAN_POINT('Ctrl Pts',(-35.6555077526845,42.812500006828,-35.6555077526845));
#13050=CARTESIAN_POINT('Ctrl Pts',(-24.3531646875,42.6041666734946,-42.1809185638422));
#13051=CARTESIAN_POINT('Ctrl Pts',(-13.0508216223155,42.3958333401613,-48.706329375));
#13052=CARTESIAN_POINT('Ctrl Pts',(1.59157945007855E-14,42.187500006828,
-48.706329375));
#13053=CARTESIAN_POINT('Ctrl Pts',(13.0508216223155,41.9791666734946,-48.706329375));
#13054=CARTESIAN_POINT('Ctrl Pts',(24.3531646875,41.7708333401613,-42.1809185638422));
#13055=CARTESIAN_POINT('Ctrl Pts',(35.6555077526845,41.562500006828,-35.6555077526845));
#13056=CARTESIAN_POINT('Ctrl Pts',(42.1809185638422,41.3541666734946,-24.3531646875));
#13057=CARTESIAN_POINT('Ctrl Pts',(48.706329375,41.1458333401613,-13.0508216223155));
#13058=CARTESIAN_POINT('Ctrl Pts',(48.706329375,40.937500006828,1.293339198242E-14));
#13059=CARTESIAN_POINT('Ctrl Pts',(48.706329375,40.7291666734946,13.0508216223155));
#13060=CARTESIAN_POINT('Ctrl Pts',(42.1809185638422,40.5208333401613,24.3531646875));
#13061=CARTESIAN_POINT('Ctrl Pts',(35.6555077526845,40.312500006828,35.6555077526845));
#13062=CARTESIAN_POINT('Ctrl Pts',(24.3531646875,40.1041666734946,42.1809185638422));
#13063=CARTESIAN_POINT('Ctrl Pts',(13.0508216223155,39.8958333401613,48.706329375));
#13064=CARTESIAN_POINT('Ctrl Pts',(-9.95098946405443E-15,39.687500006828,
48.706329375));
#13065=CARTESIAN_POINT('Ctrl Pts',(-13.0508216223155,39.4791666734946,48.706329375));
#13066=CARTESIAN_POINT('Ctrl Pts',(-24.3531646875,39.2708333401613,42.1809185638423));
#13067=CARTESIAN_POINT('Ctrl Pts',(-35.6555077526845,39.062500006828,35.6555077526845));
#13068=CARTESIAN_POINT('Ctrl Pts',(-42.1809185638422,38.8541666734946,24.3531646875));
#13069=CARTESIAN_POINT('Ctrl Pts',(-48.706329375,38.6458333401613,13.0508216223155));
#13070=CARTESIAN_POINT('Ctrl Pts',(-48.706329375,38.437500006828,-1.8898197019151E-14));
#13071=CARTESIAN_POINT('Ctrl Pts',(-48.706329375,38.2291666734946,-13.0508216223155));
#13072=CARTESIAN_POINT('Ctrl Pts',(-42.1809185638422,38.0208333401613,-24.3531646875));
#13073=CARTESIAN_POINT('Ctrl Pts',(-35.6555077526845,37.812500006828,-35.6555077526845));
#13074=CARTESIAN_POINT('Ctrl Pts',(-24.3531646875,37.6041666734946,-42.1809185638422));
#13075=CARTESIAN_POINT('Ctrl Pts',(-13.0508216223155,37.3958333401613,-48.706329375));
#13076=CARTESIAN_POINT('Ctrl Pts',(1.59157945007855E-14,37.187500006828,
-48.706329375));
#13077=CARTESIAN_POINT('Ctrl Pts',(13.0508216223155,36.9791666734946,-48.706329375));
#13078=CARTESIAN_POINT('Ctrl Pts',(24.3531646875,36.7708333401613,-42.1809185638422));
#13079=CARTESIAN_POINT('Ctrl Pts',(35.6555077526845,36.562500006828,-35.6555077526845));
#13080=CARTESIAN_POINT('Ctrl Pts',(42.1809185638422,36.3541666734946,-24.3531646875));
#13081=CARTESIAN_POINT('Ctrl Pts',(48.706329375,36.1458333401613,-13.0508216223155));
#13082=CARTESIAN_POINT('Ctrl Pts',(48.706329375,35.937500006828,1.293339198242E-14));
#13083=CARTESIAN_POINT('Ctrl Pts',(48.706329375,35.7291666734946,13.0508216223155));
#13084=CARTESIAN_POINT('Ctrl Pts',(42.1809185638422,35.5208333401613,24.3531646875));
#13085=CARTESIAN_POINT('Ctrl Pts',(35.6555077526845,35.312500006828,35.6555077526845));
#13086=CARTESIAN_POINT('Ctrl Pts',(24.3531646875,35.1041666734946,42.1809185638422));
#13087=CARTESIAN_POINT('Ctrl Pts',(13.0508216223155,34.8958333401613,48.706329375));
#13088=CARTESIAN_POINT('Ctrl Pts',(-9.95098946405443E-15,34.687500006828,
48.706329375));
#13089=CARTESIAN_POINT('Ctrl Pts',(-13.0508216223155,34.4791666734946,48.706329375));
#13090=CARTESIAN_POINT('Ctrl Pts',(-24.3531646875,34.2708333401613,42.1809185638423));
#13091=CARTESIAN_POINT('Ctrl Pts',(-35.6555077526845,34.062500006828,35.6555077526845));
#13092=CARTESIAN_POINT('Ctrl Pts',(-42.1809185638422,33.8541666734946,24.3531646875));
#13093=CARTESIAN_POINT('Ctrl Pts',(-48.706329375,33.6458333401613,13.0508216223155));
#13094=CARTESIAN_POINT('Ctrl Pts',(-48.706329375,33.437500006828,-1.8898197019151E-14));
#13095=CARTESIAN_POINT('Ctrl Pts',(-48.706329375,33.2291666734946,-13.0508216223155));
#13096=CARTESIAN_POINT('Ctrl Pts',(-42.1809185638422,33.0208333401613,-24.3531646875));
#13097=CARTESIAN_POINT('Ctrl Pts',(-35.6555077526845,32.812500006828,-35.6555077526845));
#13098=CARTESIAN_POINT('Ctrl Pts',(-24.3531646875,32.6041666734946,-42.1809185638422));
#13099=CARTESIAN_POINT('Ctrl Pts',(-13.0508216223155,32.3958333401613,-48.706329375));
#13100=CARTESIAN_POINT('Ctrl Pts',(1.59157945007855E-14,32.187500006828,
-48.706329375));
#13101=CARTESIAN_POINT('Ctrl Pts',(13.0508216223155,31.9791666734946,-48.706329375));
#13102=CARTESIAN_POINT('Ctrl Pts',(24.3531646875,31.7708333401613,-42.1809185638422));
#13103=CARTESIAN_POINT('Ctrl Pts',(35.6555077526845,31.562500006828,-35.6555077526845));
#13104=CARTESIAN_POINT('Ctrl Pts',(42.1809185638422,31.3541666734946,-24.3531646875));
#13105=CARTESIAN_POINT('Ctrl Pts',(48.706329375,31.1458333401613,-13.0508216223155));
#13106=CARTESIAN_POINT('Ctrl Pts',(48.706329375,30.937500006828,1.293339198242E-14));
#13107=CARTESIAN_POINT('Ctrl Pts',(48.706329375,30.7291666734946,13.0508216223155));
#13108=CARTESIAN_POINT('Ctrl Pts',(42.1809185638422,30.5208333401613,24.3531646875));
#13109=CARTESIAN_POINT('Ctrl Pts',(35.6555077526845,30.312500006828,35.6555077526845));
#13110=CARTESIAN_POINT('Ctrl Pts',(24.3531646875,30.1041666734946,42.1809185638422));
#13111=CARTESIAN_POINT('Ctrl Pts',(13.0508216223155,29.8958333401613,48.706329375));
#13112=CARTESIAN_POINT('Ctrl Pts',(-9.95098946405443E-15,29.687500006828,
48.706329375));
#13113=CARTESIAN_POINT('Ctrl Pts',(-13.0508216223155,29.4791666734946,48.706329375));
#13114=CARTESIAN_POINT('Ctrl Pts',(-24.3531646875,29.2708333401613,42.1809185638423));
#13115=CARTESIAN_POINT('Ctrl Pts',(-35.6555077526845,29.062500006828,35.6555077526845));
#13116=CARTESIAN_POINT('Ctrl Pts',(-42.1809185638422,28.8541666734946,24.3531646875));
#13117=CARTESIAN_POINT('Ctrl Pts',(-48.706329375,28.6458333401613,13.0508216223155));
#13118=CARTESIAN_POINT('Ctrl Pts',(-48.706329375,28.437500006828,-1.8898197019151E-14));
#13119=CARTESIAN_POINT('Ctrl Pts',(-46.,60.,0.));
#13120=CARTESIAN_POINT('Ctrl Pts',(-46.,59.7916666666667,-12.3256628518316));
#13121=CARTESIAN_POINT('Ctrl Pts',(-39.8371685740842,59.5833333333333,-23.));
#13122=CARTESIAN_POINT('Ctrl Pts',(-33.6743371481684,59.375,-33.6743371481684));
#13123=CARTESIAN_POINT('Ctrl Pts',(-23.,59.1666666666667,-39.8371685740842));
#13124=CARTESIAN_POINT('Ctrl Pts',(-12.3256628518317,58.9583333333333,-46.));
#13125=CARTESIAN_POINT('Ctrl Pts',(-2.81668763803891E-15,58.75,-46.));
#13126=CARTESIAN_POINT('Ctrl Pts',(12.3256628518316,58.5416666666667,-46.));
#13127=CARTESIAN_POINT('Ctrl Pts',(23.,58.3333333333333,-39.8371685740842));
#13128=CARTESIAN_POINT('Ctrl Pts',(33.6743371481683,58.125,-33.6743371481684));
#13129=CARTESIAN_POINT('Ctrl Pts',(39.8371685740842,57.9166666666667,-23.));
#13130=CARTESIAN_POINT('Ctrl Pts',(46.,57.7083333333333,-12.3256628518317));
#13131=CARTESIAN_POINT('Ctrl Pts',(46.,57.5,-5.63337527607782E-15));
#13132=CARTESIAN_POINT('Ctrl Pts',(46.,57.2916666666667,12.3256628518316));
#13133=CARTESIAN_POINT('Ctrl Pts',(39.8371685740842,57.0833333333333,23.));
#13134=CARTESIAN_POINT('Ctrl Pts',(33.6743371481684,56.875,33.6743371481683));
#13135=CARTESIAN_POINT('Ctrl Pts',(23.,56.6666666666667,39.8371685740842));
#13136=CARTESIAN_POINT('Ctrl Pts',(12.3256628518317,56.4583333333333,46.));
#13137=CARTESIAN_POINT('Ctrl Pts',(8.45006291411674E-15,56.25,46.));
#13138=CARTESIAN_POINT('Ctrl Pts',(-12.3256628518316,56.0416666666667,46.));
#13139=CARTESIAN_POINT('Ctrl Pts',(-23.,55.8333333333333,39.8371685740842));
#13140=CARTESIAN_POINT('Ctrl Pts',(-33.6743371481683,55.625,33.6743371481684));
#13141=CARTESIAN_POINT('Ctrl Pts',(-39.8371685740842,55.4166666666667,23.));
#13142=CARTESIAN_POINT('Ctrl Pts',(-46.,55.2083333333333,12.3256628518317));
#13143=CARTESIAN_POINT('Ctrl Pts',(-46.,55.,0.));
#13144=CARTESIAN_POINT('Ctrl Pts',(-46.,54.7916666666667,-12.3256628518316));
#13145=CARTESIAN_POINT('Ctrl Pts',(-39.8371685740842,54.5833333333333,-23.));
#13146=CARTESIAN_POINT('Ctrl Pts',(-33.6743371481684,54.375,-33.6743371481684));
#13147=CARTESIAN_POINT('Ctrl Pts',(-23.,54.1666666666667,-39.8371685740842));
#13148=CARTESIAN_POINT('Ctrl Pts',(-12.3256628518317,53.9583333333333,-46.));
#13149=CARTESIAN_POINT('Ctrl Pts',(-2.81668763803891E-15,53.75,-46.));
#13150=CARTESIAN_POINT('Ctrl Pts',(12.3256628518316,53.5416666666667,-46.));
#13151=CARTESIAN_POINT('Ctrl Pts',(23.,53.3333333333333,-39.8371685740842));
#13152=CARTESIAN_POINT('Ctrl Pts',(33.6743371481683,53.125,-33.6743371481684));
#13153=CARTESIAN_POINT('Ctrl Pts',(39.8371685740842,52.9166666666667,-23.));
#13154=CARTESIAN_POINT('Ctrl Pts',(46.,52.7083333333333,-12.3256628518317));
#13155=CARTESIAN_POINT('Ctrl Pts',(46.,52.5,-5.63337527607782E-15));
#13156=CARTESIAN_POINT('Ctrl Pts',(46.,52.2916666666667,12.3256628518316));
#13157=CARTESIAN_POINT('Ctrl Pts',(39.8371685740842,52.0833333333333,23.));
#13158=CARTESIAN_POINT('Ctrl Pts',(33.6743371481684,51.875,33.6743371481683));
#13159=CARTESIAN_POINT('Ctrl Pts',(23.,51.6666666666667,39.8371685740842));
#13160=CARTESIAN_POINT('Ctrl Pts',(12.3256628518317,51.4583333333333,46.));
#13161=CARTESIAN_POINT('Ctrl Pts',(8.45006291411674E-15,51.25,46.));
#13162=CARTESIAN_POINT('Ctrl Pts',(-12.3256628518316,51.0416666666667,46.));
#13163=CARTESIAN_POINT('Ctrl Pts',(-23.,50.8333333333333,39.8371685740842));
#13164=CARTESIAN_POINT('Ctrl Pts',(-33.6743371481683,50.625,33.6743371481684));
#13165=CARTESIAN_POINT('Ctrl Pts',(-39.8371685740842,50.4166666666667,23.));
#13166=CARTESIAN_POINT('Ctrl Pts',(-46.,50.2083333333333,12.3256628518317));
#13167=CARTESIAN_POINT('Ctrl Pts',(-46.,50.,0.));
#13168=CARTESIAN_POINT('Ctrl Pts',(-46.,49.7916666666667,-12.3256628518316));
#13169=CARTESIAN_POINT('Ctrl Pts',(-39.8371685740842,49.5833333333333,-23.));
#13170=CARTESIAN_POINT('Ctrl Pts',(-33.6743371481684,49.375,-33.6743371481684));
#13171=CARTESIAN_POINT('Ctrl Pts',(-23.,49.1666666666667,-39.8371685740842));
#13172=CARTESIAN_POINT('Ctrl Pts',(-12.3256628518317,48.9583333333333,-46.));
#13173=CARTESIAN_POINT('Ctrl Pts',(-2.81668763803891E-15,48.75,-46.));
#13174=CARTESIAN_POINT('Ctrl Pts',(12.3256628518316,48.5416666666667,-46.));
#13175=CARTESIAN_POINT('Ctrl Pts',(23.,48.3333333333333,-39.8371685740842));
#13176=CARTESIAN_POINT('Ctrl Pts',(33.6743371481683,48.125,-33.6743371481684));
#13177=CARTESIAN_POINT('Ctrl Pts',(39.8371685740842,47.9166666666667,-23.));
#13178=CARTESIAN_POINT('Ctrl Pts',(46.,47.7083333333333,-12.3256628518317));
#13179=CARTESIAN_POINT('Ctrl Pts',(46.,47.5,-5.63337527607782E-15));
#13180=CARTESIAN_POINT('Ctrl Pts',(46.,47.2916666666667,12.3256628518316));
#13181=CARTESIAN_POINT('Ctrl Pts',(39.8371685740842,47.0833333333333,23.));
#13182=CARTESIAN_POINT('Ctrl Pts',(33.6743371481684,46.875,33.6743371481683));
#13183=CARTESIAN_POINT('Ctrl Pts',(23.,46.6666666666667,39.8371685740842));
#13184=CARTESIAN_POINT('Ctrl Pts',(12.3256628518317,46.4583333333333,46.));
#13185=CARTESIAN_POINT('Ctrl Pts',(8.45006291411674E-15,46.25,46.));
#13186=CARTESIAN_POINT('Ctrl Pts',(-12.3256628518316,46.0416666666667,46.));
#13187=CARTESIAN_POINT('Ctrl Pts',(-23.,45.8333333333333,39.8371685740842));
#13188=CARTESIAN_POINT('Ctrl Pts',(-33.6743371481683,45.625,33.6743371481684));
#13189=CARTESIAN_POINT('Ctrl Pts',(-39.8371685740842,45.4166666666667,23.));
#13190=CARTESIAN_POINT('Ctrl Pts',(-46.,45.2083333333333,12.3256628518317));
#13191=CARTESIAN_POINT('Ctrl Pts',(-46.,45.,0.));
#13192=CARTESIAN_POINT('Ctrl Pts',(-46.,44.7916666666667,-12.3256628518316));
#13193=CARTESIAN_POINT('Ctrl Pts',(-39.8371685740842,44.5833333333333,-23.));
#13194=CARTESIAN_POINT('Ctrl Pts',(-33.6743371481684,44.375,-33.6743371481684));
#13195=CARTESIAN_POINT('Ctrl Pts',(-23.,44.1666666666667,-39.8371685740842));
#13196=CARTESIAN_POINT('Ctrl Pts',(-12.3256628518317,43.9583333333333,-46.));
#13197=CARTESIAN_POINT('Ctrl Pts',(-2.81668763803891E-15,43.75,-46.));
#13198=CARTESIAN_POINT('Ctrl Pts',(12.3256628518316,43.5416666666667,-46.));
#13199=CARTESIAN_POINT('Ctrl Pts',(23.,43.3333333333333,-39.8371685740842));
#13200=CARTESIAN_POINT('Ctrl Pts',(33.6743371481683,43.125,-33.6743371481684));
#13201=CARTESIAN_POINT('Ctrl Pts',(39.8371685740842,42.9166666666667,-23.));
#13202=CARTESIAN_POINT('Ctrl Pts',(46.,42.7083333333333,-12.3256628518317));
#13203=CARTESIAN_POINT('Ctrl Pts',(46.,42.5,-5.63337527607782E-15));
#13204=CARTESIAN_POINT('Ctrl Pts',(46.,42.2916666666667,12.3256628518316));
#13205=CARTESIAN_POINT('Ctrl Pts',(39.8371685740842,42.0833333333333,23.));
#13206=CARTESIAN_POINT('Ctrl Pts',(33.6743371481684,41.875,33.6743371481683));
#13207=CARTESIAN_POINT('Ctrl Pts',(23.,41.6666666666667,39.8371685740842));
#13208=CARTESIAN_POINT('Ctrl Pts',(12.3256628518317,41.4583333333333,46.));
#13209=CARTESIAN_POINT('Ctrl Pts',(8.45006291411674E-15,41.25,46.));
#13210=CARTESIAN_POINT('Ctrl Pts',(-12.3256628518316,41.0416666666667,46.));
#13211=CARTESIAN_POINT('Ctrl Pts',(-23.,40.8333333333333,39.8371685740842));
#13212=CARTESIAN_POINT('Ctrl Pts',(-33.6743371481683,40.625,33.6743371481684));
#13213=CARTESIAN_POINT('Ctrl Pts',(-39.8371685740842,40.4166666666667,23.));
#13214=CARTESIAN_POINT('Ctrl Pts',(-46.,40.2083333333333,12.3256628518317));
#13215=CARTESIAN_POINT('Ctrl Pts',(-46.,40.,0.));
#13216=CARTESIAN_POINT('Ctrl Pts',(-46.,39.7916666666667,-12.3256628518316));
#13217=CARTESIAN_POINT('Ctrl Pts',(-39.8371685740842,39.5833333333333,-23.));
#13218=CARTESIAN_POINT('Ctrl Pts',(-33.6743371481684,39.375,-33.6743371481684));
#13219=CARTESIAN_POINT('Ctrl Pts',(-23.,39.1666666666667,-39.8371685740842));
#13220=CARTESIAN_POINT('Ctrl Pts',(-12.3256628518317,38.9583333333333,-46.));
#13221=CARTESIAN_POINT('Ctrl Pts',(-2.81668763803891E-15,38.75,-46.));
#13222=CARTESIAN_POINT('Ctrl Pts',(12.3256628518316,38.5416666666667,-46.));
#13223=CARTESIAN_POINT('Ctrl Pts',(23.,38.3333333333333,-39.8371685740842));
#13224=CARTESIAN_POINT('Ctrl Pts',(33.6743371481683,38.125,-33.6743371481684));
#13225=CARTESIAN_POINT('Ctrl Pts',(39.8371685740842,37.9166666666667,-23.));
#13226=CARTESIAN_POINT('Ctrl Pts',(46.,37.7083333333333,-12.3256628518317));
#13227=CARTESIAN_POINT('Ctrl Pts',(46.,37.5,-5.63337527607782E-15));
#13228=CARTESIAN_POINT('Ctrl Pts',(46.,37.2916666666667,12.3256628518316));
#13229=CARTESIAN_POINT('Ctrl Pts',(39.8371685740842,37.0833333333333,23.));
#13230=CARTESIAN_POINT('Ctrl Pts',(33.6743371481684,36.875,33.6743371481683));
#13231=CARTESIAN_POINT('Ctrl Pts',(23.,36.6666666666667,39.8371685740842));
#13232=CARTESIAN_POINT('Ctrl Pts',(12.3256628518317,36.4583333333333,46.));
#13233=CARTESIAN_POINT('Ctrl Pts',(8.45006291411674E-15,36.25,46.));
#13234=CARTESIAN_POINT('Ctrl Pts',(-12.3256628518316,36.0416666666667,46.));
#13235=CARTESIAN_POINT('Ctrl Pts',(-23.,35.8333333333333,39.8371685740842));
#13236=CARTESIAN_POINT('Ctrl Pts',(-33.6743371481683,35.625,33.6743371481684));
#13237=CARTESIAN_POINT('Ctrl Pts',(-39.8371685740842,35.4166666666667,23.));
#13238=CARTESIAN_POINT('Ctrl Pts',(-46.,35.2083333333333,12.3256628518317));
#13239=CARTESIAN_POINT('Ctrl Pts',(-46.,35.,0.));
#13240=CARTESIAN_POINT('Ctrl Pts',(-46.,34.7916666666667,-12.3256628518316));
#13241=CARTESIAN_POINT('Ctrl Pts',(-39.8371685740842,34.5833333333333,-23.));
#13242=CARTESIAN_POINT('Ctrl Pts',(-33.6743371481684,34.375,-33.6743371481684));
#13243=CARTESIAN_POINT('Ctrl Pts',(-23.,34.1666666666667,-39.8371685740842));
#13244=CARTESIAN_POINT('Ctrl Pts',(-12.3256628518317,33.9583333333333,-46.));
#13245=CARTESIAN_POINT('Ctrl Pts',(-2.81668763803891E-15,33.75,-46.));
#13246=CARTESIAN_POINT('Ctrl Pts',(12.3256628518316,33.5416666666667,-46.));
#13247=CARTESIAN_POINT('Ctrl Pts',(23.,33.3333333333333,-39.8371685740842));
#13248=CARTESIAN_POINT('Ctrl Pts',(33.6743371481683,33.125,-33.6743371481684));
#13249=CARTESIAN_POINT('Ctrl Pts',(39.8371685740842,32.9166666666667,-23.));
#13250=CARTESIAN_POINT('Ctrl Pts',(46.,32.7083333333333,-12.3256628518317));
#13251=CARTESIAN_POINT('Ctrl Pts',(46.,32.5,-5.63337527607782E-15));
#13252=CARTESIAN_POINT('Ctrl Pts',(46.,32.2916666666667,12.3256628518316));
#13253=CARTESIAN_POINT('Ctrl Pts',(39.8371685740842,32.0833333333333,23.));
#13254=CARTESIAN_POINT('Ctrl Pts',(33.6743371481684,31.875,33.6743371481683));
#13255=CARTESIAN_POINT('Ctrl Pts',(23.,31.6666666666667,39.8371685740842));
#13256=CARTESIAN_POINT('Ctrl Pts',(12.3256628518317,31.4583333333333,46.));
#13257=CARTESIAN_POINT('Ctrl Pts',(8.45006291411674E-15,31.25,46.));
#13258=CARTESIAN_POINT('Ctrl Pts',(-12.3256628518316,31.0416666666667,46.));
#13259=CARTESIAN_POINT('Ctrl Pts',(-23.,30.8333333333333,39.8371685740842));
#13260=CARTESIAN_POINT('Ctrl Pts',(-33.6743371481683,30.625,33.6743371481684));
#13261=CARTESIAN_POINT('Ctrl Pts',(-39.8371685740842,30.4166666666667,23.));
#13262=CARTESIAN_POINT('Ctrl Pts',(-46.,30.2083333333333,12.3256628518317));
#13263=CARTESIAN_POINT('Ctrl Pts',(-46.,30.,0.));
#13264=CARTESIAN_POINT('Ctrl Pts',(45.7957082162897,42.5741208584476,-4.3304859967968));
#13265=CARTESIAN_POINT('Ctrl Pts',(46.027322302781,42.4406160752063,-4.3304859967968));
#13266=CARTESIAN_POINT('Ctrl Pts',(46.4905476657727,42.1736016336912,-4.33048599679655));
#13267=CARTESIAN_POINT('Ctrl Pts',(46.9537676533565,41.9065778670208,-4.33048599679681));
#13268=CARTESIAN_POINT('Ctrl Pts',(47.6280672732221,41.5178683162597,-4.33048599679681));
#13269=CARTESIAN_POINT('Ctrl Pts',(48.0707534890442,41.2626647328764,-4.33048599679679));
#13270=CARTESIAN_POINT('Ctrl Pts',(48.5134353784344,41.0074536451604,-4.33048599679679));
#13271=CARTESIAN_POINT('Ctrl Pts',(3.61292728433798,42.1292520480093,-48.5721450795008));
#13272=CARTESIAN_POINT('Ctrl Pts',(3.61292728433798,42.2624339185675,-48.3403451622818));
#13273=CARTESIAN_POINT('Ctrl Pts',(3.61292728433799,42.395608829009,-48.1085412459393));
#13274=CARTESIAN_POINT('Ctrl Pts',(3.61292728433799,42.6619441142016,-47.6449250631479));
#13275=CARTESIAN_POINT('Ctrl Pts',(3.61292728433793,42.7951044891727,-47.4131127965212));
#13276=CARTESIAN_POINT('Ctrl Pts',(3.61292728433793,42.9282572703914,-47.1812961682826));
#13277=CARTESIAN_POINT('Ctrl Pts',(3.61292728433793,43.1816295626638,-46.7401795055578));
#13278=CARTESIAN_POINT('Ctrl Pts',(3.61292728433795,43.4349743764897,-46.2990470581854));
#13279=CARTESIAN_POINT('Ctrl Pts',(3.61292728433795,43.688289262853,-45.8578974271399));
#13280=CARTESIAN_POINT('Ctrl Pts',(-48.706329375,58.437500006828,-1.8898197019151E-14));
#13281=CARTESIAN_POINT('Ctrl Pts',(-48.706329375,58.2291666734946,-13.0508216223155));
#13282=CARTESIAN_POINT('Ctrl Pts',(-42.1809185638422,58.0208333401613,-24.3531646875));
#13283=CARTESIAN_POINT('Ctrl Pts',(-35.6555077526845,57.812500006828,-35.6555077526845));
#13284=CARTESIAN_POINT('Ctrl Pts',(-24.3531646875,57.6041666734946,-42.1809185638422));
#13285=CARTESIAN_POINT('Ctrl Pts',(-13.0508216223155,57.3958333401613,-48.706329375));
#13286=CARTESIAN_POINT('Ctrl Pts',(1.59157945007855E-14,57.187500006828,
-48.706329375));
#13287=CARTESIAN_POINT('Ctrl Pts',(13.0508216223155,56.9791666734946,-48.706329375));
#13288=CARTESIAN_POINT('Ctrl Pts',(24.3531646875,56.7708333401613,-42.1809185638422));
#13289=CARTESIAN_POINT('Ctrl Pts',(35.6555077526845,56.562500006828,-35.6555077526845));
#13290=CARTESIAN_POINT('Ctrl Pts',(42.1809185638422,56.3541666734946,-24.3531646875));
#13291=CARTESIAN_POINT('Ctrl Pts',(48.706329375,56.1458333401613,-13.0508216223155));
#13292=CARTESIAN_POINT('Ctrl Pts',(48.706329375,55.937500006828,1.293339198242E-14));
#13293=CARTESIAN_POINT('Ctrl Pts',(48.706329375,55.7291666734946,13.0508216223155));
#13294=CARTESIAN_POINT('Ctrl Pts',(42.1809185638422,55.5208333401613,24.3531646875));
#13295=CARTESIAN_POINT('Ctrl Pts',(35.6555077526845,55.312500006828,35.6555077526845));
#13296=CARTESIAN_POINT('Ctrl Pts',(24.3531646875,55.1041666734946,42.1809185638422));
#13297=CARTESIAN_POINT('Ctrl Pts',(13.0508216223155,54.8958333401613,48.706329375));
#13298=CARTESIAN_POINT('Ctrl Pts',(-9.95098946405443E-15,54.687500006828,
48.706329375));
#13299=CARTESIAN_POINT('Ctrl Pts',(-13.0508216223155,54.4791666734946,48.706329375));
#13300=CARTESIAN_POINT('Ctrl Pts',(-24.3531646875,54.2708333401613,42.1809185638423));
#13301=CARTESIAN_POINT('Ctrl Pts',(-35.6555077526845,54.062500006828,35.6555077526845));
#13302=CARTESIAN_POINT('Ctrl Pts',(-42.1809185638422,53.8541666734946,24.3531646875));
#13303=CARTESIAN_POINT('Ctrl Pts',(-48.706329375,53.6458333401613,13.0508216223155));
#13304=CARTESIAN_POINT('Ctrl Pts',(-48.706329375,53.437500006828,-1.8898197019151E-14));
#13305=CARTESIAN_POINT('Ctrl Pts',(-48.706329375,53.2291666734946,-13.0508216223155));
#13306=CARTESIAN_POINT('Ctrl Pts',(-42.1809185638422,53.0208333401613,-24.3531646875));
#13307=CARTESIAN_POINT('Ctrl Pts',(-35.6555077526845,52.812500006828,-35.6555077526845));
#13308=CARTESIAN_POINT('Ctrl Pts',(-24.3531646875,52.6041666734946,-42.1809185638422));
#13309=CARTESIAN_POINT('Ctrl Pts',(-13.0508216223155,52.3958333401613,-48.706329375));
#13310=CARTESIAN_POINT('Ctrl Pts',(1.59157945007855E-14,52.187500006828,
-48.706329375));
#13311=CARTESIAN_POINT('Ctrl Pts',(13.0508216223155,51.9791666734946,-48.706329375));
#13312=CARTESIAN_POINT('Ctrl Pts',(24.3531646875,51.7708333401613,-42.1809185638422));
#13313=CARTESIAN_POINT('Ctrl Pts',(35.6555077526845,51.562500006828,-35.6555077526845));
#13314=CARTESIAN_POINT('Ctrl Pts',(42.1809185638422,51.3541666734946,-24.3531646875));
#13315=CARTESIAN_POINT('Ctrl Pts',(48.706329375,51.1458333401613,-13.0508216223155));
#13316=CARTESIAN_POINT('Ctrl Pts',(48.706329375,50.937500006828,1.293339198242E-14));
#13317=CARTESIAN_POINT('Ctrl Pts',(48.706329375,50.7291666734946,13.0508216223155));
#13318=CARTESIAN_POINT('Ctrl Pts',(42.1809185638422,50.5208333401613,24.3531646875));
#13319=CARTESIAN_POINT('Ctrl Pts',(35.6555077526845,50.312500006828,35.6555077526845));
#13320=CARTESIAN_POINT('Ctrl Pts',(24.3531646875,50.1041666734946,42.1809185638422));
#13321=CARTESIAN_POINT('Ctrl Pts',(13.0508216223155,49.8958333401613,48.706329375));
#13322=CARTESIAN_POINT('Ctrl Pts',(-9.95098946405443E-15,49.687500006828,
48.706329375));
#13323=CARTESIAN_POINT('Ctrl Pts',(-13.0508216223155,49.4791666734946,48.706329375));
#13324=CARTESIAN_POINT('Ctrl Pts',(-24.3531646875,49.2708333401613,42.1809185638423));
#13325=CARTESIAN_POINT('Ctrl Pts',(-35.6555077526845,49.062500006828,35.6555077526845));
#13326=CARTESIAN_POINT('Ctrl Pts',(-42.1809185638422,48.8541666734946,24.3531646875));
#13327=CARTESIAN_POINT('Ctrl Pts',(-48.706329375,48.6458333401613,13.0508216223155));
#13328=CARTESIAN_POINT('Ctrl Pts',(-48.706329375,48.437500006828,-1.8898197019151E-14));
#13329=CARTESIAN_POINT('Ctrl Pts',(-48.706329375,48.2291666734946,-13.0508216223155));
#13330=CARTESIAN_POINT('Ctrl Pts',(-42.1809185638422,48.0208333401613,-24.3531646875));
#13331=CARTESIAN_POINT('Ctrl Pts',(-35.6555077526845,47.812500006828,-35.6555077526845));
#13332=CARTESIAN_POINT('Ctrl Pts',(-24.3531646875,47.6041666734946,-42.1809185638422));
#13333=CARTESIAN_POINT('Ctrl Pts',(-13.0508216223155,47.3958333401613,-48.706329375));
#13334=CARTESIAN_POINT('Ctrl Pts',(1.59157945007855E-14,47.187500006828,
-48.706329375));
#13335=CARTESIAN_POINT('Ctrl Pts',(13.0508216223155,46.9791666734946,-48.706329375));
#13336=CARTESIAN_POINT('Ctrl Pts',(24.3531646875,46.7708333401613,-42.1809185638422));
#13337=CARTESIAN_POINT('Ctrl Pts',(35.6555077526845,46.562500006828,-35.6555077526845));
#13338=CARTESIAN_POINT('Ctrl Pts',(42.1809185638422,46.3541666734946,-24.3531646875));
#13339=CARTESIAN_POINT('Ctrl Pts',(48.706329375,46.1458333401613,-13.0508216223155));
#13340=CARTESIAN_POINT('Ctrl Pts',(48.706329375,45.937500006828,1.293339198242E-14));
#13341=CARTESIAN_POINT('Ctrl Pts',(48.706329375,45.7291666734946,13.0508216223155));
#13342=CARTESIAN_POINT('Ctrl Pts',(42.1809185638422,45.5208333401613,24.3531646875));
#13343=CARTESIAN_POINT('Ctrl Pts',(35.6555077526845,45.312500006828,35.6555077526845));
#13344=CARTESIAN_POINT('Ctrl Pts',(24.3531646875,45.1041666734946,42.1809185638422));
#13345=CARTESIAN_POINT('Ctrl Pts',(13.0508216223155,44.8958333401613,48.706329375));
#13346=CARTESIAN_POINT('Ctrl Pts',(-9.95098946405443E-15,44.687500006828,
48.706329375));
#13347=CARTESIAN_POINT('Ctrl Pts',(-13.0508216223155,44.4791666734946,48.706329375));
#13348=CARTESIAN_POINT('Ctrl Pts',(-24.3531646875,44.2708333401613,42.1809185638423));
#13349=CARTESIAN_POINT('Ctrl Pts',(-35.6555077526845,44.062500006828,35.6555077526845));
#13350=CARTESIAN_POINT('Ctrl Pts',(-42.1809185638422,43.8541666734946,24.3531646875));
#13351=CARTESIAN_POINT('Ctrl Pts',(-48.706329375,43.6458333401613,13.0508216223155));
#13352=CARTESIAN_POINT('Ctrl Pts',(-48.706329375,43.437500006828,-1.8898197019151E-14));
#13353=CARTESIAN_POINT('Ctrl Pts',(-48.706329375,43.2291666734946,-13.0508216223155));
#13354=CARTESIAN_POINT('Ctrl Pts',(-42.1809185638422,43.0208333401613,-24.3531646875));
#13355=CARTESIAN_POINT('Ctrl Pts',(-35.6555077526845,42.812500006828,-35.6555077526845));
#13356=CARTESIAN_POINT('Ctrl Pts',(-24.3531646875,42.6041666734946,-42.1809185638422));
#13357=CARTESIAN_POINT('Ctrl Pts',(-13.0508216223155,42.3958333401613,-48.706329375));
#13358=CARTESIAN_POINT('Ctrl Pts',(1.59157945007855E-14,42.187500006828,
-48.706329375));
#13359=CARTESIAN_POINT('Ctrl Pts',(13.0508216223155,41.9791666734946,-48.706329375));
#13360=CARTESIAN_POINT('Ctrl Pts',(24.3531646875,41.7708333401613,-42.1809185638422));
#13361=CARTESIAN_POINT('Ctrl Pts',(35.6555077526845,41.562500006828,-35.6555077526845));
#13362=CARTESIAN_POINT('Ctrl Pts',(42.1809185638422,41.3541666734946,-24.3531646875));
#13363=CARTESIAN_POINT('Ctrl Pts',(48.706329375,41.1458333401613,-13.0508216223155));
#13364=CARTESIAN_POINT('Ctrl Pts',(48.706329375,40.937500006828,1.293339198242E-14));
#13365=CARTESIAN_POINT('Ctrl Pts',(48.706329375,40.7291666734946,13.0508216223155));
#13366=CARTESIAN_POINT('Ctrl Pts',(42.1809185638422,40.5208333401613,24.3531646875));
#13367=CARTESIAN_POINT('Ctrl Pts',(35.6555077526845,40.312500006828,35.6555077526845));
#13368=CARTESIAN_POINT('Ctrl Pts',(24.3531646875,40.1041666734946,42.1809185638422));
#13369=CARTESIAN_POINT('Ctrl Pts',(13.0508216223155,39.8958333401613,48.706329375));
#13370=CARTESIAN_POINT('Ctrl Pts',(-9.95098946405443E-15,39.687500006828,
48.706329375));
#13371=CARTESIAN_POINT('Ctrl Pts',(-13.0508216223155,39.4791666734946,48.706329375));
#13372=CARTESIAN_POINT('Ctrl Pts',(-24.3531646875,39.2708333401613,42.1809185638423));
#13373=CARTESIAN_POINT('Ctrl Pts',(-35.6555077526845,39.062500006828,35.6555077526845));
#13374=CARTESIAN_POINT('Ctrl Pts',(-42.1809185638422,38.8541666734946,24.3531646875));
#13375=CARTESIAN_POINT('Ctrl Pts',(-48.706329375,38.6458333401613,13.0508216223155));
#13376=CARTESIAN_POINT('Ctrl Pts',(-48.706329375,38.437500006828,-1.8898197019151E-14));
#13377=CARTESIAN_POINT('Ctrl Pts',(-48.706329375,38.2291666734946,-13.0508216223155));
#13378=CARTESIAN_POINT('Ctrl Pts',(-42.1809185638422,38.0208333401613,-24.3531646875));
#13379=CARTESIAN_POINT('Ctrl Pts',(-35.6555077526845,37.812500006828,-35.6555077526845));
#13380=CARTESIAN_POINT('Ctrl Pts',(-24.3531646875,37.6041666734946,-42.1809185638422));
#13381=CARTESIAN_POINT('Ctrl Pts',(-13.0508216223155,37.3958333401613,-48.706329375));
#13382=CARTESIAN_POINT('Ctrl Pts',(1.59157945007855E-14,37.187500006828,
-48.706329375));
#13383=CARTESIAN_POINT('Ctrl Pts',(13.0508216223155,36.9791666734946,-48.706329375));
#13384=CARTESIAN_POINT('Ctrl Pts',(24.3531646875,36.7708333401613,-42.1809185638422));
#13385=CARTESIAN_POINT('Ctrl Pts',(35.6555077526845,36.562500006828,-35.6555077526845));
#13386=CARTESIAN_POINT('Ctrl Pts',(42.1809185638422,36.3541666734946,-24.3531646875));
#13387=CARTESIAN_POINT('Ctrl Pts',(48.706329375,36.1458333401613,-13.0508216223155));
#13388=CARTESIAN_POINT('Ctrl Pts',(48.706329375,35.937500006828,1.293339198242E-14));
#13389=CARTESIAN_POINT('Ctrl Pts',(48.706329375,35.7291666734946,13.0508216223155));
#13390=CARTESIAN_POINT('Ctrl Pts',(42.1809185638422,35.5208333401613,24.3531646875));
#13391=CARTESIAN_POINT('Ctrl Pts',(35.6555077526845,35.312500006828,35.6555077526845));
#13392=CARTESIAN_POINT('Ctrl Pts',(24.3531646875,35.1041666734946,42.1809185638422));
#13393=CARTESIAN_POINT('Ctrl Pts',(13.0508216223155,34.8958333401613,48.706329375));
#13394=CARTESIAN_POINT('Ctrl Pts',(-9.95098946405443E-15,34.687500006828,
48.706329375));
#13395=CARTESIAN_POINT('Ctrl Pts',(-13.0508216223155,34.4791666734946,48.706329375));
#13396=CARTESIAN_POINT('Ctrl Pts',(-24.3531646875,34.2708333401613,42.1809185638423));
#13397=CARTESIAN_POINT('Ctrl Pts',(-35.6555077526845,34.062500006828,35.6555077526845));
#13398=CARTESIAN_POINT('Ctrl Pts',(-42.1809185638422,33.8541666734946,24.3531646875));
#13399=CARTESIAN_POINT('Ctrl Pts',(-48.706329375,33.6458333401613,13.0508216223155));
#13400=CARTESIAN_POINT('Ctrl Pts',(-48.706329375,33.437500006828,-1.8898197019151E-14));
#13401=CARTESIAN_POINT('Ctrl Pts',(-48.706329375,33.2291666734946,-13.0508216223155));
#13402=CARTESIAN_POINT('Ctrl Pts',(-42.1809185638422,33.0208333401613,-24.3531646875));
#13403=CARTESIAN_POINT('Ctrl Pts',(-35.6555077526845,32.812500006828,-35.6555077526845));
#13404=CARTESIAN_POINT('Ctrl Pts',(-24.3531646875,32.6041666734946,-42.1809185638422));
#13405=CARTESIAN_POINT('Ctrl Pts',(-13.0508216223155,32.3958333401613,-48.706329375));
#13406=CARTESIAN_POINT('Ctrl Pts',(1.59157945007855E-14,32.187500006828,
-48.706329375));
#13407=CARTESIAN_POINT('Ctrl Pts',(13.0508216223155,31.9791666734946,-48.706329375));
#13408=CARTESIAN_POINT('Ctrl Pts',(24.3531646875,31.7708333401613,-42.1809185638422));
#13409=CARTESIAN_POINT('Ctrl Pts',(35.6555077526845,31.562500006828,-35.6555077526845));
#13410=CARTESIAN_POINT('Ctrl Pts',(42.1809185638422,31.3541666734946,-24.3531646875));
#13411=CARTESIAN_POINT('Ctrl Pts',(48.706329375,31.1458333401613,-13.0508216223155));
#13412=CARTESIAN_POINT('Ctrl Pts',(48.706329375,30.937500006828,1.293339198242E-14));
#13413=CARTESIAN_POINT('Ctrl Pts',(48.706329375,30.7291666734946,13.0508216223155));
#13414=CARTESIAN_POINT('Ctrl Pts',(42.1809185638422,30.5208333401613,24.3531646875));
#13415=CARTESIAN_POINT('Ctrl Pts',(35.6555077526845,30.312500006828,35.6555077526845));
#13416=CARTESIAN_POINT('Ctrl Pts',(24.3531646875,30.1041666734946,42.1809185638422));
#13417=CARTESIAN_POINT('Ctrl Pts',(13.0508216223155,29.8958333401613,48.706329375));
#13418=CARTESIAN_POINT('Ctrl Pts',(-9.95098946405443E-15,29.687500006828,
48.706329375));
#13419=CARTESIAN_POINT('Ctrl Pts',(-13.0508216223155,29.4791666734946,48.706329375));
#13420=CARTESIAN_POINT('Ctrl Pts',(-24.3531646875,29.2708333401613,42.1809185638423));
#13421=CARTESIAN_POINT('Ctrl Pts',(-35.6555077526845,29.062500006828,35.6555077526845));
#13422=CARTESIAN_POINT('Ctrl Pts',(-42.1809185638422,28.8541666734946,24.3531646875));
#13423=CARTESIAN_POINT('Ctrl Pts',(-48.706329375,28.6458333401613,13.0508216223155));
#13424=CARTESIAN_POINT('Ctrl Pts',(-48.706329375,28.437500006828,-1.8898197019151E-14));
#13425=CARTESIAN_POINT('Ctrl Pts',(-46.,60.,0.));
#13426=CARTESIAN_POINT('Ctrl Pts',(-46.,59.7916666666667,-12.3256628518316));
#13427=CARTESIAN_POINT('Ctrl Pts',(-39.8371685740842,59.5833333333333,-23.));
#13428=CARTESIAN_POINT('Ctrl Pts',(-33.6743371481684,59.375,-33.6743371481684));
#13429=CARTESIAN_POINT('Ctrl Pts',(-23.,59.1666666666667,-39.8371685740842));
#13430=CARTESIAN_POINT('Ctrl Pts',(-12.3256628518317,58.9583333333333,-46.));
#13431=CARTESIAN_POINT('Ctrl Pts',(-2.81668763803891E-15,58.75,-46.));
#13432=CARTESIAN_POINT('Ctrl Pts',(12.3256628518316,58.5416666666667,-46.));
#13433=CARTESIAN_POINT('Ctrl Pts',(23.,58.3333333333333,-39.8371685740842));
#13434=CARTESIAN_POINT('Ctrl Pts',(33.6743371481683,58.125,-33.6743371481684));
#13435=CARTESIAN_POINT('Ctrl Pts',(39.8371685740842,57.9166666666667,-23.));
#13436=CARTESIAN_POINT('Ctrl Pts',(46.,57.7083333333333,-12.3256628518317));
#13437=CARTESIAN_POINT('Ctrl Pts',(46.,57.5,-5.63337527607782E-15));
#13438=CARTESIAN_POINT('Ctrl Pts',(46.,57.2916666666667,12.3256628518316));
#13439=CARTESIAN_POINT('Ctrl Pts',(39.8371685740842,57.0833333333333,23.));
#13440=CARTESIAN_POINT('Ctrl Pts',(33.6743371481684,56.875,33.6743371481683));
#13441=CARTESIAN_POINT('Ctrl Pts',(23.,56.6666666666667,39.8371685740842));
#13442=CARTESIAN_POINT('Ctrl Pts',(12.3256628518317,56.4583333333333,46.));
#13443=CARTESIAN_POINT('Ctrl Pts',(8.45006291411674E-15,56.25,46.));
#13444=CARTESIAN_POINT('Ctrl Pts',(-12.3256628518316,56.0416666666667,46.));
#13445=CARTESIAN_POINT('Ctrl Pts',(-23.,55.8333333333333,39.8371685740842));
#13446=CARTESIAN_POINT('Ctrl Pts',(-33.6743371481683,55.625,33.6743371481684));
#13447=CARTESIAN_POINT('Ctrl Pts',(-39.8371685740842,55.4166666666667,23.));
#13448=CARTESIAN_POINT('Ctrl Pts',(-46.,55.2083333333333,12.3256628518317));
#13449=CARTESIAN_POINT('Ctrl Pts',(-46.,55.,0.));
#13450=CARTESIAN_POINT('Ctrl Pts',(-46.,54.7916666666667,-12.3256628518316));
#13451=CARTESIAN_POINT('Ctrl Pts',(-39.8371685740842,54.5833333333333,-23.));
#13452=CARTESIAN_POINT('Ctrl Pts',(-33.6743371481684,54.375,-33.6743371481684));
#13453=CARTESIAN_POINT('Ctrl Pts',(-23.,54.1666666666667,-39.8371685740842));
#13454=CARTESIAN_POINT('Ctrl Pts',(-12.3256628518317,53.9583333333333,-46.));
#13455=CARTESIAN_POINT('Ctrl Pts',(-2.81668763803891E-15,53.75,-46.));
#13456=CARTESIAN_POINT('Ctrl Pts',(12.3256628518316,53.5416666666667,-46.));
#13457=CARTESIAN_POINT('Ctrl Pts',(23.,53.3333333333333,-39.8371685740842));
#13458=CARTESIAN_POINT('Ctrl Pts',(33.6743371481683,53.125,-33.6743371481684));
#13459=CARTESIAN_POINT('Ctrl Pts',(39.8371685740842,52.9166666666667,-23.));
#13460=CARTESIAN_POINT('Ctrl Pts',(46.,52.7083333333333,-12.3256628518317));
#13461=CARTESIAN_POINT('Ctrl Pts',(46.,52.5,-5.63337527607782E-15));
#13462=CARTESIAN_POINT('Ctrl Pts',(46.,52.2916666666667,12.3256628518316));
#13463=CARTESIAN_POINT('Ctrl Pts',(39.8371685740842,52.0833333333333,23.));
#13464=CARTESIAN_POINT('Ctrl Pts',(33.6743371481684,51.875,33.6743371481683));
#13465=CARTESIAN_POINT('Ctrl Pts',(23.,51.6666666666667,39.8371685740842));
#13466=CARTESIAN_POINT('Ctrl Pts',(12.3256628518317,51.4583333333333,46.));
#13467=CARTESIAN_POINT('Ctrl Pts',(8.45006291411674E-15,51.25,46.));
#13468=CARTESIAN_POINT('Ctrl Pts',(-12.3256628518316,51.0416666666667,46.));
#13469=CARTESIAN_POINT('Ctrl Pts',(-23.,50.8333333333333,39.8371685740842));
#13470=CARTESIAN_POINT('Ctrl Pts',(-33.6743371481683,50.625,33.6743371481684));
#13471=CARTESIAN_POINT('Ctrl Pts',(-39.8371685740842,50.4166666666667,23.));
#13472=CARTESIAN_POINT('Ctrl Pts',(-46.,50.2083333333333,12.3256628518317));
#13473=CARTESIAN_POINT('Ctrl Pts',(-46.,50.,0.));
#13474=CARTESIAN_POINT('Ctrl Pts',(-46.,49.7916666666667,-12.3256628518316));
#13475=CARTESIAN_POINT('Ctrl Pts',(-39.8371685740842,49.5833333333333,-23.));
#13476=CARTESIAN_POINT('Ctrl Pts',(-33.6743371481684,49.375,-33.6743371481684));
#13477=CARTESIAN_POINT('Ctrl Pts',(-23.,49.1666666666667,-39.8371685740842));
#13478=CARTESIAN_POINT('Ctrl Pts',(-12.3256628518317,48.9583333333333,-46.));
#13479=CARTESIAN_POINT('Ctrl Pts',(-2.81668763803891E-15,48.75,-46.));
#13480=CARTESIAN_POINT('Ctrl Pts',(12.3256628518316,48.5416666666667,-46.));
#13481=CARTESIAN_POINT('Ctrl Pts',(23.,48.3333333333333,-39.8371685740842));
#13482=CARTESIAN_POINT('Ctrl Pts',(33.6743371481683,48.125,-33.6743371481684));
#13483=CARTESIAN_POINT('Ctrl Pts',(39.8371685740842,47.9166666666667,-23.));
#13484=CARTESIAN_POINT('Ctrl Pts',(46.,47.7083333333333,-12.3256628518317));
#13485=CARTESIAN_POINT('Ctrl Pts',(46.,47.5,-5.63337527607782E-15));
#13486=CARTESIAN_POINT('Ctrl Pts',(46.,47.2916666666667,12.3256628518316));
#13487=CARTESIAN_POINT('Ctrl Pts',(39.8371685740842,47.0833333333333,23.));
#13488=CARTESIAN_POINT('Ctrl Pts',(33.6743371481684,46.875,33.6743371481683));
#13489=CARTESIAN_POINT('Ctrl Pts',(23.,46.6666666666667,39.8371685740842));
#13490=CARTESIAN_POINT('Ctrl Pts',(12.3256628518317,46.4583333333333,46.));
#13491=CARTESIAN_POINT('Ctrl Pts',(8.45006291411674E-15,46.25,46.));
#13492=CARTESIAN_POINT('Ctrl Pts',(-12.3256628518316,46.0416666666667,46.));
#13493=CARTESIAN_POINT('Ctrl Pts',(-23.,45.8333333333333,39.8371685740842));
#13494=CARTESIAN_POINT('Ctrl Pts',(-33.6743371481683,45.625,33.6743371481684));
#13495=CARTESIAN_POINT('Ctrl Pts',(-39.8371685740842,45.4166666666667,23.));
#13496=CARTESIAN_POINT('Ctrl Pts',(-46.,45.2083333333333,12.3256628518317));
#13497=CARTESIAN_POINT('Ctrl Pts',(-46.,45.,0.));
#13498=CARTESIAN_POINT('Ctrl Pts',(-46.,44.7916666666667,-12.3256628518316));
#13499=CARTESIAN_POINT('Ctrl Pts',(-39.8371685740842,44.5833333333333,-23.));
#13500=CARTESIAN_POINT('Ctrl Pts',(-33.6743371481684,44.375,-33.6743371481684));
#13501=CARTESIAN_POINT('Ctrl Pts',(-23.,44.1666666666667,-39.8371685740842));
#13502=CARTESIAN_POINT('Ctrl Pts',(-12.3256628518317,43.9583333333333,-46.));
#13503=CARTESIAN_POINT('Ctrl Pts',(-2.81668763803891E-15,43.75,-46.));
#13504=CARTESIAN_POINT('Ctrl Pts',(12.3256628518316,43.5416666666667,-46.));
#13505=CARTESIAN_POINT('Ctrl Pts',(23.,43.3333333333333,-39.8371685740842));
#13506=CARTESIAN_POINT('Ctrl Pts',(33.6743371481683,43.125,-33.6743371481684));
#13507=CARTESIAN_POINT('Ctrl Pts',(39.8371685740842,42.9166666666667,-23.));
#13508=CARTESIAN_POINT('Ctrl Pts',(46.,42.7083333333333,-12.3256628518317));
#13509=CARTESIAN_POINT('Ctrl Pts',(46.,42.5,-5.63337527607782E-15));
#13510=CARTESIAN_POINT('Ctrl Pts',(46.,42.2916666666667,12.3256628518316));
#13511=CARTESIAN_POINT('Ctrl Pts',(39.8371685740842,42.0833333333333,23.));
#13512=CARTESIAN_POINT('Ctrl Pts',(33.6743371481684,41.875,33.6743371481683));
#13513=CARTESIAN_POINT('Ctrl Pts',(23.,41.6666666666667,39.8371685740842));
#13514=CARTESIAN_POINT('Ctrl Pts',(12.3256628518317,41.4583333333333,46.));
#13515=CARTESIAN_POINT('Ctrl Pts',(8.45006291411674E-15,41.25,46.));
#13516=CARTESIAN_POINT('Ctrl Pts',(-12.3256628518316,41.0416666666667,46.));
#13517=CARTESIAN_POINT('Ctrl Pts',(-23.,40.8333333333333,39.8371685740842));
#13518=CARTESIAN_POINT('Ctrl Pts',(-33.6743371481683,40.625,33.6743371481684));
#13519=CARTESIAN_POINT('Ctrl Pts',(-39.8371685740842,40.4166666666667,23.));
#13520=CARTESIAN_POINT('Ctrl Pts',(-46.,40.2083333333333,12.3256628518317));
#13521=CARTESIAN_POINT('Ctrl Pts',(-46.,40.,0.));
#13522=CARTESIAN_POINT('Ctrl Pts',(-46.,39.7916666666667,-12.3256628518316));
#13523=CARTESIAN_POINT('Ctrl Pts',(-39.8371685740842,39.5833333333333,-23.));
#13524=CARTESIAN_POINT('Ctrl Pts',(-33.6743371481684,39.375,-33.6743371481684));
#13525=CARTESIAN_POINT('Ctrl Pts',(-23.,39.1666666666667,-39.8371685740842));
#13526=CARTESIAN_POINT('Ctrl Pts',(-12.3256628518317,38.9583333333333,-46.));
#13527=CARTESIAN_POINT('Ctrl Pts',(-2.81668763803891E-15,38.75,-46.));
#13528=CARTESIAN_POINT('Ctrl Pts',(12.3256628518316,38.5416666666667,-46.));
#13529=CARTESIAN_POINT('Ctrl Pts',(23.,38.3333333333333,-39.8371685740842));
#13530=CARTESIAN_POINT('Ctrl Pts',(33.6743371481683,38.125,-33.6743371481684));
#13531=CARTESIAN_POINT('Ctrl Pts',(39.8371685740842,37.9166666666667,-23.));
#13532=CARTESIAN_POINT('Ctrl Pts',(46.,37.7083333333333,-12.3256628518317));
#13533=CARTESIAN_POINT('Ctrl Pts',(46.,37.5,-5.63337527607782E-15));
#13534=CARTESIAN_POINT('Ctrl Pts',(46.,37.2916666666667,12.3256628518316));
#13535=CARTESIAN_POINT('Ctrl Pts',(39.8371685740842,37.0833333333333,23.));
#13536=CARTESIAN_POINT('Ctrl Pts',(33.6743371481684,36.875,33.6743371481683));
#13537=CARTESIAN_POINT('Ctrl Pts',(23.,36.6666666666667,39.8371685740842));
#13538=CARTESIAN_POINT('Ctrl Pts',(12.3256628518317,36.4583333333333,46.));
#13539=CARTESIAN_POINT('Ctrl Pts',(8.45006291411674E-15,36.25,46.));
#13540=CARTESIAN_POINT('Ctrl Pts',(-12.3256628518316,36.0416666666667,46.));
#13541=CARTESIAN_POINT('Ctrl Pts',(-23.,35.8333333333333,39.8371685740842));
#13542=CARTESIAN_POINT('Ctrl Pts',(-33.6743371481683,35.625,33.6743371481684));
#13543=CARTESIAN_POINT('Ctrl Pts',(-39.8371685740842,35.4166666666667,23.));
#13544=CARTESIAN_POINT('Ctrl Pts',(-46.,35.2083333333333,12.3256628518317));
#13545=CARTESIAN_POINT('Ctrl Pts',(-46.,35.,0.));
#13546=CARTESIAN_POINT('Ctrl Pts',(-46.,34.7916666666667,-12.3256628518316));
#13547=CARTESIAN_POINT('Ctrl Pts',(-39.8371685740842,34.5833333333333,-23.));
#13548=CARTESIAN_POINT('Ctrl Pts',(-33.6743371481684,34.375,-33.6743371481684));
#13549=CARTESIAN_POINT('Ctrl Pts',(-23.,34.1666666666667,-39.8371685740842));
#13550=CARTESIAN_POINT('Ctrl Pts',(-12.3256628518317,33.9583333333333,-46.));
#13551=CARTESIAN_POINT('Ctrl Pts',(-2.81668763803891E-15,33.75,-46.));
#13552=CARTESIAN_POINT('Ctrl Pts',(12.3256628518316,33.5416666666667,-46.));
#13553=CARTESIAN_POINT('Ctrl Pts',(23.,33.3333333333333,-39.8371685740842));
#13554=CARTESIAN_POINT('Ctrl Pts',(33.6743371481683,33.125,-33.6743371481684));
#13555=CARTESIAN_POINT('Ctrl Pts',(39.8371685740842,32.9166666666667,-23.));
#13556=CARTESIAN_POINT('Ctrl Pts',(46.,32.7083333333333,-12.3256628518317));
#13557=CARTESIAN_POINT('Ctrl Pts',(46.,32.5,-5.63337527607782E-15));
#13558=CARTESIAN_POINT('Ctrl Pts',(46.,32.2916666666667,12.3256628518316));
#13559=CARTESIAN_POINT('Ctrl Pts',(39.8371685740842,32.0833333333333,23.));
#13560=CARTESIAN_POINT('Ctrl Pts',(33.6743371481684,31.875,33.6743371481683));
#13561=CARTESIAN_POINT('Ctrl Pts',(23.,31.6666666666667,39.8371685740842));
#13562=CARTESIAN_POINT('Ctrl Pts',(12.3256628518317,31.4583333333333,46.));
#13563=CARTESIAN_POINT('Ctrl Pts',(8.45006291411674E-15,31.25,46.));
#13564=CARTESIAN_POINT('Ctrl Pts',(-12.3256628518316,31.0416666666667,46.));
#13565=CARTESIAN_POINT('Ctrl Pts',(-23.,30.8333333333333,39.8371685740842));
#13566=CARTESIAN_POINT('Ctrl Pts',(-33.6743371481683,30.625,33.6743371481684));
#13567=CARTESIAN_POINT('Ctrl Pts',(-39.8371685740842,30.4166666666667,23.));
#13568=CARTESIAN_POINT('Ctrl Pts',(-46.,30.2083333333333,12.3256628518317));
#13569=CARTESIAN_POINT('Ctrl Pts',(-46.,30.,0.));
#13570=CARTESIAN_POINT('Ctrl Pts',(48.5725845633798,40.8793483229262,3.60701400320329));
#13571=CARTESIAN_POINT('Ctrl Pts',(48.3407853679392,41.0125314497137,3.60701400320329));
#13572=CARTESIAN_POINT('Ctrl Pts',(48.1089821836664,41.1457076343819,3.60701400320328));
#13573=CARTESIAN_POINT('Ctrl Pts',(47.6453674864979,41.4120455056142,3.60701400320328));
#13574=CARTESIAN_POINT('Ctrl Pts',(47.4135559734254,41.5452071923974,3.60701400320326));
#13575=CARTESIAN_POINT('Ctrl Pts',(47.1817401099609,41.6783613050641,3.60701400320326));
#13576=CARTESIAN_POINT('Ctrl Pts',(46.7406305897488,41.9317328641751,3.60701400320326));
#13577=CARTESIAN_POINT('Ctrl Pts',(46.2995053259033,42.1850770165972,3.60701400320326));
#13578=CARTESIAN_POINT('Ctrl Pts',(45.858362923034,42.438391319744,3.60701400320326));
#13579=CARTESIAN_POINT('Ctrl Pts',(3.61292728433799,41.311710737147,45.8578974271399));
#13580=CARTESIAN_POINT('Ctrl Pts',(3.61292728433799,41.178117727701,46.089460636719));
#13581=CARTESIAN_POINT('Ctrl Pts',(3.61292728433786,40.9109294856547,46.5525857733052));
#13582=CARTESIAN_POINT('Ctrl Pts',(3.61292728433808,40.6437369897944,47.0157084557285));
#13583=CARTESIAN_POINT('Ctrl Pts',(3.61292728433808,40.2553460757966,47.6888965792834));
#13584=CARTESIAN_POINT('Ctrl Pts',(3.61292728433799,40.0005487265709,48.1305218136162));
#13585=CARTESIAN_POINT('Ctrl Pts',(3.61292728433799,39.7457479656467,48.5721450795008));
#13586=CARTESIAN_POINT('Ctrl Pts',(-48.706329375,58.437500006828,-1.8898197019151E-14));
#13587=CARTESIAN_POINT('Ctrl Pts',(-48.706329375,58.2291666734946,-13.0508216223155));
#13588=CARTESIAN_POINT('Ctrl Pts',(-42.1809185638422,58.0208333401613,-24.3531646875));
#13589=CARTESIAN_POINT('Ctrl Pts',(-35.6555077526845,57.812500006828,-35.6555077526845));
#13590=CARTESIAN_POINT('Ctrl Pts',(-24.3531646875,57.6041666734946,-42.1809185638422));
#13591=CARTESIAN_POINT('Ctrl Pts',(-13.0508216223155,57.3958333401613,-48.706329375));
#13592=CARTESIAN_POINT('Ctrl Pts',(1.59157945007855E-14,57.187500006828,
-48.706329375));
#13593=CARTESIAN_POINT('Ctrl Pts',(13.0508216223155,56.9791666734946,-48.706329375));
#13594=CARTESIAN_POINT('Ctrl Pts',(24.3531646875,56.7708333401613,-42.1809185638422));
#13595=CARTESIAN_POINT('Ctrl Pts',(35.6555077526845,56.562500006828,-35.6555077526845));
#13596=CARTESIAN_POINT('Ctrl Pts',(42.1809185638422,56.3541666734946,-24.3531646875));
#13597=CARTESIAN_POINT('Ctrl Pts',(48.706329375,56.1458333401613,-13.0508216223155));
#13598=CARTESIAN_POINT('Ctrl Pts',(48.706329375,55.937500006828,1.293339198242E-14));
#13599=CARTESIAN_POINT('Ctrl Pts',(48.706329375,55.7291666734946,13.0508216223155));
#13600=CARTESIAN_POINT('Ctrl Pts',(42.1809185638422,55.5208333401613,24.3531646875));
#13601=CARTESIAN_POINT('Ctrl Pts',(35.6555077526845,55.312500006828,35.6555077526845));
#13602=CARTESIAN_POINT('Ctrl Pts',(24.3531646875,55.1041666734946,42.1809185638422));
#13603=CARTESIAN_POINT('Ctrl Pts',(13.0508216223155,54.8958333401613,48.706329375));
#13604=CARTESIAN_POINT('Ctrl Pts',(-9.95098946405443E-15,54.687500006828,
48.706329375));
#13605=CARTESIAN_POINT('Ctrl Pts',(-13.0508216223155,54.4791666734946,48.706329375));
#13606=CARTESIAN_POINT('Ctrl Pts',(-24.3531646875,54.2708333401613,42.1809185638423));
#13607=CARTESIAN_POINT('Ctrl Pts',(-35.6555077526845,54.062500006828,35.6555077526845));
#13608=CARTESIAN_POINT('Ctrl Pts',(-42.1809185638422,53.8541666734946,24.3531646875));
#13609=CARTESIAN_POINT('Ctrl Pts',(-48.706329375,53.6458333401613,13.0508216223155));
#13610=CARTESIAN_POINT('Ctrl Pts',(-48.706329375,53.437500006828,-1.8898197019151E-14));
#13611=CARTESIAN_POINT('Ctrl Pts',(-48.706329375,53.2291666734946,-13.0508216223155));
#13612=CARTESIAN_POINT('Ctrl Pts',(-42.1809185638422,53.0208333401613,-24.3531646875));
#13613=CARTESIAN_POINT('Ctrl Pts',(-35.6555077526845,52.812500006828,-35.6555077526845));
#13614=CARTESIAN_POINT('Ctrl Pts',(-24.3531646875,52.6041666734946,-42.1809185638422));
#13615=CARTESIAN_POINT('Ctrl Pts',(-13.0508216223155,52.3958333401613,-48.706329375));
#13616=CARTESIAN_POINT('Ctrl Pts',(1.59157945007855E-14,52.187500006828,
-48.706329375));
#13617=CARTESIAN_POINT('Ctrl Pts',(13.0508216223155,51.9791666734946,-48.706329375));
#13618=CARTESIAN_POINT('Ctrl Pts',(24.3531646875,51.7708333401613,-42.1809185638422));
#13619=CARTESIAN_POINT('Ctrl Pts',(35.6555077526845,51.562500006828,-35.6555077526845));
#13620=CARTESIAN_POINT('Ctrl Pts',(42.1809185638422,51.3541666734946,-24.3531646875));
#13621=CARTESIAN_POINT('Ctrl Pts',(48.706329375,51.1458333401613,-13.0508216223155));
#13622=CARTESIAN_POINT('Ctrl Pts',(48.706329375,50.937500006828,1.293339198242E-14));
#13623=CARTESIAN_POINT('Ctrl Pts',(48.706329375,50.7291666734946,13.0508216223155));
#13624=CARTESIAN_POINT('Ctrl Pts',(42.1809185638422,50.5208333401613,24.3531646875));
#13625=CARTESIAN_POINT('Ctrl Pts',(35.6555077526845,50.312500006828,35.6555077526845));
#13626=CARTESIAN_POINT('Ctrl Pts',(24.3531646875,50.1041666734946,42.1809185638422));
#13627=CARTESIAN_POINT('Ctrl Pts',(13.0508216223155,49.8958333401613,48.706329375));
#13628=CARTESIAN_POINT('Ctrl Pts',(-9.95098946405443E-15,49.687500006828,
48.706329375));
#13629=CARTESIAN_POINT('Ctrl Pts',(-13.0508216223155,49.4791666734946,48.706329375));
#13630=CARTESIAN_POINT('Ctrl Pts',(-24.3531646875,49.2708333401613,42.1809185638423));
#13631=CARTESIAN_POINT('Ctrl Pts',(-35.6555077526845,49.062500006828,35.6555077526845));
#13632=CARTESIAN_POINT('Ctrl Pts',(-42.1809185638422,48.8541666734946,24.3531646875));
#13633=CARTESIAN_POINT('Ctrl Pts',(-48.706329375,48.6458333401613,13.0508216223155));
#13634=CARTESIAN_POINT('Ctrl Pts',(-48.706329375,48.437500006828,-1.8898197019151E-14));
#13635=CARTESIAN_POINT('Ctrl Pts',(-48.706329375,48.2291666734946,-13.0508216223155));
#13636=CARTESIAN_POINT('Ctrl Pts',(-42.1809185638422,48.0208333401613,-24.3531646875));
#13637=CARTESIAN_POINT('Ctrl Pts',(-35.6555077526845,47.812500006828,-35.6555077526845));
#13638=CARTESIAN_POINT('Ctrl Pts',(-24.3531646875,47.6041666734946,-42.1809185638422));
#13639=CARTESIAN_POINT('Ctrl Pts',(-13.0508216223155,47.3958333401613,-48.706329375));
#13640=CARTESIAN_POINT('Ctrl Pts',(1.59157945007855E-14,47.187500006828,
-48.706329375));
#13641=CARTESIAN_POINT('Ctrl Pts',(13.0508216223155,46.9791666734946,-48.706329375));
#13642=CARTESIAN_POINT('Ctrl Pts',(24.3531646875,46.7708333401613,-42.1809185638422));
#13643=CARTESIAN_POINT('Ctrl Pts',(35.6555077526845,46.562500006828,-35.6555077526845));
#13644=CARTESIAN_POINT('Ctrl Pts',(42.1809185638422,46.3541666734946,-24.3531646875));
#13645=CARTESIAN_POINT('Ctrl Pts',(48.706329375,46.1458333401613,-13.0508216223155));
#13646=CARTESIAN_POINT('Ctrl Pts',(48.706329375,45.937500006828,1.293339198242E-14));
#13647=CARTESIAN_POINT('Ctrl Pts',(48.706329375,45.7291666734946,13.0508216223155));
#13648=CARTESIAN_POINT('Ctrl Pts',(42.1809185638422,45.5208333401613,24.3531646875));
#13649=CARTESIAN_POINT('Ctrl Pts',(35.6555077526845,45.312500006828,35.6555077526845));
#13650=CARTESIAN_POINT('Ctrl Pts',(24.3531646875,45.1041666734946,42.1809185638422));
#13651=CARTESIAN_POINT('Ctrl Pts',(13.0508216223155,44.8958333401613,48.706329375));
#13652=CARTESIAN_POINT('Ctrl Pts',(-9.95098946405443E-15,44.687500006828,
48.706329375));
#13653=CARTESIAN_POINT('Ctrl Pts',(-13.0508216223155,44.4791666734946,48.706329375));
#13654=CARTESIAN_POINT('Ctrl Pts',(-24.3531646875,44.2708333401613,42.1809185638423));
#13655=CARTESIAN_POINT('Ctrl Pts',(-35.6555077526845,44.062500006828,35.6555077526845));
#13656=CARTESIAN_POINT('Ctrl Pts',(-42.1809185638422,43.8541666734946,24.3531646875));
#13657=CARTESIAN_POINT('Ctrl Pts',(-48.706329375,43.6458333401613,13.0508216223155));
#13658=CARTESIAN_POINT('Ctrl Pts',(-48.706329375,43.437500006828,-1.8898197019151E-14));
#13659=CARTESIAN_POINT('Ctrl Pts',(-48.706329375,43.2291666734946,-13.0508216223155));
#13660=CARTESIAN_POINT('Ctrl Pts',(-42.1809185638422,43.0208333401613,-24.3531646875));
#13661=CARTESIAN_POINT('Ctrl Pts',(-35.6555077526845,42.812500006828,-35.6555077526845));
#13662=CARTESIAN_POINT('Ctrl Pts',(-24.3531646875,42.6041666734946,-42.1809185638422));
#13663=CARTESIAN_POINT('Ctrl Pts',(-13.0508216223155,42.3958333401613,-48.706329375));
#13664=CARTESIAN_POINT('Ctrl Pts',(1.59157945007855E-14,42.187500006828,
-48.706329375));
#13665=CARTESIAN_POINT('Ctrl Pts',(13.0508216223155,41.9791666734946,-48.706329375));
#13666=CARTESIAN_POINT('Ctrl Pts',(24.3531646875,41.7708333401613,-42.1809185638422));
#13667=CARTESIAN_POINT('Ctrl Pts',(35.6555077526845,41.562500006828,-35.6555077526845));
#13668=CARTESIAN_POINT('Ctrl Pts',(42.1809185638422,41.3541666734946,-24.3531646875));
#13669=CARTESIAN_POINT('Ctrl Pts',(48.706329375,41.1458333401613,-13.0508216223155));
#13670=CARTESIAN_POINT('Ctrl Pts',(48.706329375,40.937500006828,1.293339198242E-14));
#13671=CARTESIAN_POINT('Ctrl Pts',(48.706329375,40.7291666734946,13.0508216223155));
#13672=CARTESIAN_POINT('Ctrl Pts',(42.1809185638422,40.5208333401613,24.3531646875));
#13673=CARTESIAN_POINT('Ctrl Pts',(35.6555077526845,40.312500006828,35.6555077526845));
#13674=CARTESIAN_POINT('Ctrl Pts',(24.3531646875,40.1041666734946,42.1809185638422));
#13675=CARTESIAN_POINT('Ctrl Pts',(13.0508216223155,39.8958333401613,48.706329375));
#13676=CARTESIAN_POINT('Ctrl Pts',(-9.95098946405443E-15,39.687500006828,
48.706329375));
#13677=CARTESIAN_POINT('Ctrl Pts',(-13.0508216223155,39.4791666734946,48.706329375));
#13678=CARTESIAN_POINT('Ctrl Pts',(-24.3531646875,39.2708333401613,42.1809185638423));
#13679=CARTESIAN_POINT('Ctrl Pts',(-35.6555077526845,39.062500006828,35.6555077526845));
#13680=CARTESIAN_POINT('Ctrl Pts',(-42.1809185638422,38.8541666734946,24.3531646875));
#13681=CARTESIAN_POINT('Ctrl Pts',(-48.706329375,38.6458333401613,13.0508216223155));
#13682=CARTESIAN_POINT('Ctrl Pts',(-48.706329375,38.437500006828,-1.8898197019151E-14));
#13683=CARTESIAN_POINT('Ctrl Pts',(-48.706329375,38.2291666734946,-13.0508216223155));
#13684=CARTESIAN_POINT('Ctrl Pts',(-42.1809185638422,38.0208333401613,-24.3531646875));
#13685=CARTESIAN_POINT('Ctrl Pts',(-35.6555077526845,37.812500006828,-35.6555077526845));
#13686=CARTESIAN_POINT('Ctrl Pts',(-24.3531646875,37.6041666734946,-42.1809185638422));
#13687=CARTESIAN_POINT('Ctrl Pts',(-13.0508216223155,37.3958333401613,-48.706329375));
#13688=CARTESIAN_POINT('Ctrl Pts',(1.59157945007855E-14,37.187500006828,
-48.706329375));
#13689=CARTESIAN_POINT('Ctrl Pts',(13.0508216223155,36.9791666734946,-48.706329375));
#13690=CARTESIAN_POINT('Ctrl Pts',(24.3531646875,36.7708333401613,-42.1809185638422));
#13691=CARTESIAN_POINT('Ctrl Pts',(35.6555077526845,36.562500006828,-35.6555077526845));
#13692=CARTESIAN_POINT('Ctrl Pts',(42.1809185638422,36.3541666734946,-24.3531646875));
#13693=CARTESIAN_POINT('Ctrl Pts',(48.706329375,36.1458333401613,-13.0508216223155));
#13694=CARTESIAN_POINT('Ctrl Pts',(48.706329375,35.937500006828,1.293339198242E-14));
#13695=CARTESIAN_POINT('Ctrl Pts',(48.706329375,35.7291666734946,13.0508216223155));
#13696=CARTESIAN_POINT('Ctrl Pts',(42.1809185638422,35.5208333401613,24.3531646875));
#13697=CARTESIAN_POINT('Ctrl Pts',(35.6555077526845,35.312500006828,35.6555077526845));
#13698=CARTESIAN_POINT('Ctrl Pts',(24.3531646875,35.1041666734946,42.1809185638422));
#13699=CARTESIAN_POINT('Ctrl Pts',(13.0508216223155,34.8958333401613,48.706329375));
#13700=CARTESIAN_POINT('Ctrl Pts',(-9.95098946405443E-15,34.687500006828,
48.706329375));
#13701=CARTESIAN_POINT('Ctrl Pts',(-13.0508216223155,34.4791666734946,48.706329375));
#13702=CARTESIAN_POINT('Ctrl Pts',(-24.3531646875,34.2708333401613,42.1809185638423));
#13703=CARTESIAN_POINT('Ctrl Pts',(-35.6555077526845,34.062500006828,35.6555077526845));
#13704=CARTESIAN_POINT('Ctrl Pts',(-42.1809185638422,33.8541666734946,24.3531646875));
#13705=CARTESIAN_POINT('Ctrl Pts',(-48.706329375,33.6458333401613,13.0508216223155));
#13706=CARTESIAN_POINT('Ctrl Pts',(-48.706329375,33.437500006828,-1.8898197019151E-14));
#13707=CARTESIAN_POINT('Ctrl Pts',(-48.706329375,33.2291666734946,-13.0508216223155));
#13708=CARTESIAN_POINT('Ctrl Pts',(-42.1809185638422,33.0208333401613,-24.3531646875));
#13709=CARTESIAN_POINT('Ctrl Pts',(-35.6555077526845,32.812500006828,-35.6555077526845));
#13710=CARTESIAN_POINT('Ctrl Pts',(-24.3531646875,32.6041666734946,-42.1809185638422));
#13711=CARTESIAN_POINT('Ctrl Pts',(-13.0508216223155,32.3958333401613,-48.706329375));
#13712=CARTESIAN_POINT('Ctrl Pts',(1.59157945007855E-14,32.187500006828,
-48.706329375));
#13713=CARTESIAN_POINT('Ctrl Pts',(13.0508216223155,31.9791666734946,-48.706329375));
#13714=CARTESIAN_POINT('Ctrl Pts',(24.3531646875,31.7708333401613,-42.1809185638422));
#13715=CARTESIAN_POINT('Ctrl Pts',(35.6555077526845,31.562500006828,-35.6555077526845));
#13716=CARTESIAN_POINT('Ctrl Pts',(42.1809185638422,31.3541666734946,-24.3531646875));
#13717=CARTESIAN_POINT('Ctrl Pts',(48.706329375,31.1458333401613,-13.0508216223155));
#13718=CARTESIAN_POINT('Ctrl Pts',(48.706329375,30.937500006828,1.293339198242E-14));
#13719=CARTESIAN_POINT('Ctrl Pts',(48.706329375,30.7291666734946,13.0508216223155));
#13720=CARTESIAN_POINT('Ctrl Pts',(42.1809185638422,30.5208333401613,24.3531646875));
#13721=CARTESIAN_POINT('Ctrl Pts',(35.6555077526845,30.312500006828,35.6555077526845));
#13722=CARTESIAN_POINT('Ctrl Pts',(24.3531646875,30.1041666734946,42.1809185638422));
#13723=CARTESIAN_POINT('Ctrl Pts',(13.0508216223155,29.8958333401613,48.706329375));
#13724=CARTESIAN_POINT('Ctrl Pts',(-9.95098946405443E-15,29.687500006828,
48.706329375));
#13725=CARTESIAN_POINT('Ctrl Pts',(-13.0508216223155,29.4791666734946,48.706329375));
#13726=CARTESIAN_POINT('Ctrl Pts',(-24.3531646875,29.2708333401613,42.1809185638423));
#13727=CARTESIAN_POINT('Ctrl Pts',(-35.6555077526845,29.062500006828,35.6555077526845));
#13728=CARTESIAN_POINT('Ctrl Pts',(-42.1809185638422,28.8541666734946,24.3531646875));
#13729=CARTESIAN_POINT('Ctrl Pts',(-48.706329375,28.6458333401613,13.0508216223155));
#13730=CARTESIAN_POINT('Ctrl Pts',(-48.706329375,28.437500006828,-1.8898197019151E-14));
#13731=CARTESIAN_POINT('Ctrl Pts',(-46.,60.,0.));
#13732=CARTESIAN_POINT('Ctrl Pts',(-46.,59.7916666666667,-12.3256628518316));
#13733=CARTESIAN_POINT('Ctrl Pts',(-39.8371685740842,59.5833333333333,-23.));
#13734=CARTESIAN_POINT('Ctrl Pts',(-33.6743371481684,59.375,-33.6743371481684));
#13735=CARTESIAN_POINT('Ctrl Pts',(-23.,59.1666666666667,-39.8371685740842));
#13736=CARTESIAN_POINT('Ctrl Pts',(-12.3256628518317,58.9583333333333,-46.));
#13737=CARTESIAN_POINT('Ctrl Pts',(-2.81668763803891E-15,58.75,-46.));
#13738=CARTESIAN_POINT('Ctrl Pts',(12.3256628518316,58.5416666666667,-46.));
#13739=CARTESIAN_POINT('Ctrl Pts',(23.,58.3333333333333,-39.8371685740842));
#13740=CARTESIAN_POINT('Ctrl Pts',(33.6743371481683,58.125,-33.6743371481684));
#13741=CARTESIAN_POINT('Ctrl Pts',(39.8371685740842,57.9166666666667,-23.));
#13742=CARTESIAN_POINT('Ctrl Pts',(46.,57.7083333333333,-12.3256628518317));
#13743=CARTESIAN_POINT('Ctrl Pts',(46.,57.5,-5.63337527607782E-15));
#13744=CARTESIAN_POINT('Ctrl Pts',(46.,57.2916666666667,12.3256628518316));
#13745=CARTESIAN_POINT('Ctrl Pts',(39.8371685740842,57.0833333333333,23.));
#13746=CARTESIAN_POINT('Ctrl Pts',(33.6743371481684,56.875,33.6743371481683));
#13747=CARTESIAN_POINT('Ctrl Pts',(23.,56.6666666666667,39.8371685740842));
#13748=CARTESIAN_POINT('Ctrl Pts',(12.3256628518317,56.4583333333333,46.));
#13749=CARTESIAN_POINT('Ctrl Pts',(8.45006291411674E-15,56.25,46.));
#13750=CARTESIAN_POINT('Ctrl Pts',(-12.3256628518316,56.0416666666667,46.));
#13751=CARTESIAN_POINT('Ctrl Pts',(-23.,55.8333333333333,39.8371685740842));
#13752=CARTESIAN_POINT('Ctrl Pts',(-33.6743371481683,55.625,33.6743371481684));
#13753=CARTESIAN_POINT('Ctrl Pts',(-39.8371685740842,55.4166666666667,23.));
#13754=CARTESIAN_POINT('Ctrl Pts',(-46.,55.2083333333333,12.3256628518317));
#13755=CARTESIAN_POINT('Ctrl Pts',(-46.,55.,0.));
#13756=CARTESIAN_POINT('Ctrl Pts',(-46.,54.7916666666667,-12.3256628518316));
#13757=CARTESIAN_POINT('Ctrl Pts',(-39.8371685740842,54.5833333333333,-23.));
#13758=CARTESIAN_POINT('Ctrl Pts',(-33.6743371481684,54.375,-33.6743371481684));
#13759=CARTESIAN_POINT('Ctrl Pts',(-23.,54.1666666666667,-39.8371685740842));
#13760=CARTESIAN_POINT('Ctrl Pts',(-12.3256628518317,53.9583333333333,-46.));
#13761=CARTESIAN_POINT('Ctrl Pts',(-2.81668763803891E-15,53.75,-46.));
#13762=CARTESIAN_POINT('Ctrl Pts',(12.3256628518316,53.5416666666667,-46.));
#13763=CARTESIAN_POINT('Ctrl Pts',(23.,53.3333333333333,-39.8371685740842));
#13764=CARTESIAN_POINT('Ctrl Pts',(33.6743371481683,53.125,-33.6743371481684));
#13765=CARTESIAN_POINT('Ctrl Pts',(39.8371685740842,52.9166666666667,-23.));
#13766=CARTESIAN_POINT('Ctrl Pts',(46.,52.7083333333333,-12.3256628518317));
#13767=CARTESIAN_POINT('Ctrl Pts',(46.,52.5,-5.63337527607782E-15));
#13768=CARTESIAN_POINT('Ctrl Pts',(46.,52.2916666666667,12.3256628518316));
#13769=CARTESIAN_POINT('Ctrl Pts',(39.8371685740842,52.0833333333333,23.));
#13770=CARTESIAN_POINT('Ctrl Pts',(33.6743371481684,51.875,33.6743371481683));
#13771=CARTESIAN_POINT('Ctrl Pts',(23.,51.6666666666667,39.8371685740842));
#13772=CARTESIAN_POINT('Ctrl Pts',(12.3256628518317,51.4583333333333,46.));
#13773=CARTESIAN_POINT('Ctrl Pts',(8.45006291411674E-15,51.25,46.));
#13774=CARTESIAN_POINT('Ctrl Pts',(-12.3256628518316,51.0416666666667,46.));
#13775=CARTESIAN_POINT('Ctrl Pts',(-23.,50.8333333333333,39.8371685740842));
#13776=CARTESIAN_POINT('Ctrl Pts',(-33.6743371481683,50.625,33.6743371481684));
#13777=CARTESIAN_POINT('Ctrl Pts',(-39.8371685740842,50.4166666666667,23.));
#13778=CARTESIAN_POINT('Ctrl Pts',(-46.,50.2083333333333,12.3256628518317));
#13779=CARTESIAN_POINT('Ctrl Pts',(-46.,50.,0.));
#13780=CARTESIAN_POINT('Ctrl Pts',(-46.,49.7916666666667,-12.3256628518316));
#13781=CARTESIAN_POINT('Ctrl Pts',(-39.8371685740842,49.5833333333333,-23.));
#13782=CARTESIAN_POINT('Ctrl Pts',(-33.6743371481684,49.375,-33.6743371481684));
#13783=CARTESIAN_POINT('Ctrl Pts',(-23.,49.1666666666667,-39.8371685740842));
#13784=CARTESIAN_POINT('Ctrl Pts',(-12.3256628518317,48.9583333333333,-46.));
#13785=CARTESIAN_POINT('Ctrl Pts',(-2.81668763803891E-15,48.75,-46.));
#13786=CARTESIAN_POINT('Ctrl Pts',(12.3256628518316,48.5416666666667,-46.));
#13787=CARTESIAN_POINT('Ctrl Pts',(23.,48.3333333333333,-39.8371685740842));
#13788=CARTESIAN_POINT('Ctrl Pts',(33.6743371481683,48.125,-33.6743371481684));
#13789=CARTESIAN_POINT('Ctrl Pts',(39.8371685740842,47.9166666666667,-23.));
#13790=CARTESIAN_POINT('Ctrl Pts',(46.,47.7083333333333,-12.3256628518317));
#13791=CARTESIAN_POINT('Ctrl Pts',(46.,47.5,-5.63337527607782E-15));
#13792=CARTESIAN_POINT('Ctrl Pts',(46.,47.2916666666667,12.3256628518316));
#13793=CARTESIAN_POINT('Ctrl Pts',(39.8371685740842,47.0833333333333,23.));
#13794=CARTESIAN_POINT('Ctrl Pts',(33.6743371481684,46.875,33.6743371481683));
#13795=CARTESIAN_POINT('Ctrl Pts',(23.,46.6666666666667,39.8371685740842));
#13796=CARTESIAN_POINT('Ctrl Pts',(12.3256628518317,46.4583333333333,46.));
#13797=CARTESIAN_POINT('Ctrl Pts',(8.45006291411674E-15,46.25,46.));
#13798=CARTESIAN_POINT('Ctrl Pts',(-12.3256628518316,46.0416666666667,46.));
#13799=CARTESIAN_POINT('Ctrl Pts',(-23.,45.8333333333333,39.8371685740842));
#13800=CARTESIAN_POINT('Ctrl Pts',(-33.6743371481683,45.625,33.6743371481684));
#13801=CARTESIAN_POINT('Ctrl Pts',(-39.8371685740842,45.4166666666667,23.));
#13802=CARTESIAN_POINT('Ctrl Pts',(-46.,45.2083333333333,12.3256628518317));
#13803=CARTESIAN_POINT('Ctrl Pts',(-46.,45.,0.));
#13804=CARTESIAN_POINT('Ctrl Pts',(-46.,44.7916666666667,-12.3256628518316));
#13805=CARTESIAN_POINT('Ctrl Pts',(-39.8371685740842,44.5833333333333,-23.));
#13806=CARTESIAN_POINT('Ctrl Pts',(-33.6743371481684,44.375,-33.6743371481684));
#13807=CARTESIAN_POINT('Ctrl Pts',(-23.,44.1666666666667,-39.8371685740842));
#13808=CARTESIAN_POINT('Ctrl Pts',(-12.3256628518317,43.9583333333333,-46.));
#13809=CARTESIAN_POINT('Ctrl Pts',(-2.81668763803891E-15,43.75,-46.));
#13810=CARTESIAN_POINT('Ctrl Pts',(12.3256628518316,43.5416666666667,-46.));
#13811=CARTESIAN_POINT('Ctrl Pts',(23.,43.3333333333333,-39.8371685740842));
#13812=CARTESIAN_POINT('Ctrl Pts',(33.6743371481683,43.125,-33.6743371481684));
#13813=CARTESIAN_POINT('Ctrl Pts',(39.8371685740842,42.9166666666667,-23.));
#13814=CARTESIAN_POINT('Ctrl Pts',(46.,42.7083333333333,-12.3256628518317));
#13815=CARTESIAN_POINT('Ctrl Pts',(46.,42.5,-5.63337527607782E-15));
#13816=CARTESIAN_POINT('Ctrl Pts',(46.,42.2916666666667,12.3256628518316));
#13817=CARTESIAN_POINT('Ctrl Pts',(39.8371685740842,42.0833333333333,23.));
#13818=CARTESIAN_POINT('Ctrl Pts',(33.6743371481684,41.875,33.6743371481683));
#13819=CARTESIAN_POINT('Ctrl Pts',(23.,41.6666666666667,39.8371685740842));
#13820=CARTESIAN_POINT('Ctrl Pts',(12.3256628518317,41.4583333333333,46.));
#13821=CARTESIAN_POINT('Ctrl Pts',(8.45006291411674E-15,41.25,46.));
#13822=CARTESIAN_POINT('Ctrl Pts',(-12.3256628518316,41.0416666666667,46.));
#13823=CARTESIAN_POINT('Ctrl Pts',(-23.,40.8333333333333,39.8371685740842));
#13824=CARTESIAN_POINT('Ctrl Pts',(-33.6743371481683,40.625,33.6743371481684));
#13825=CARTESIAN_POINT('Ctrl Pts',(-39.8371685740842,40.4166666666667,23.));
#13826=CARTESIAN_POINT('Ctrl Pts',(-46.,40.2083333333333,12.3256628518317));
#13827=CARTESIAN_POINT('Ctrl Pts',(-46.,40.,0.));
#13828=CARTESIAN_POINT('Ctrl Pts',(-46.,39.7916666666667,-12.3256628518316));
#13829=CARTESIAN_POINT('Ctrl Pts',(-39.8371685740842,39.5833333333333,-23.));
#13830=CARTESIAN_POINT('Ctrl Pts',(-33.6743371481684,39.375,-33.6743371481684));
#13831=CARTESIAN_POINT('Ctrl Pts',(-23.,39.1666666666667,-39.8371685740842));
#13832=CARTESIAN_POINT('Ctrl Pts',(-12.3256628518317,38.9583333333333,-46.));
#13833=CARTESIAN_POINT('Ctrl Pts',(-2.81668763803891E-15,38.75,-46.));
#13834=CARTESIAN_POINT('Ctrl Pts',(12.3256628518316,38.5416666666667,-46.));
#13835=CARTESIAN_POINT('Ctrl Pts',(23.,38.3333333333333,-39.8371685740842));
#13836=CARTESIAN_POINT('Ctrl Pts',(33.6743371481683,38.125,-33.6743371481684));
#13837=CARTESIAN_POINT('Ctrl Pts',(39.8371685740842,37.9166666666667,-23.));
#13838=CARTESIAN_POINT('Ctrl Pts',(46.,37.7083333333333,-12.3256628518317));
#13839=CARTESIAN_POINT('Ctrl Pts',(46.,37.5,-5.63337527607782E-15));
#13840=CARTESIAN_POINT('Ctrl Pts',(46.,37.2916666666667,12.3256628518316));
#13841=CARTESIAN_POINT('Ctrl Pts',(39.8371685740842,37.0833333333333,23.));
#13842=CARTESIAN_POINT('Ctrl Pts',(33.6743371481684,36.875,33.6743371481683));
#13843=CARTESIAN_POINT('Ctrl Pts',(23.,36.6666666666667,39.8371685740842));
#13844=CARTESIAN_POINT('Ctrl Pts',(12.3256628518317,36.4583333333333,46.));
#13845=CARTESIAN_POINT('Ctrl Pts',(8.45006291411674E-15,36.25,46.));
#13846=CARTESIAN_POINT('Ctrl Pts',(-12.3256628518316,36.0416666666667,46.));
#13847=CARTESIAN_POINT('Ctrl Pts',(-23.,35.8333333333333,39.8371685740842));
#13848=CARTESIAN_POINT('Ctrl Pts',(-33.6743371481683,35.625,33.6743371481684));
#13849=CARTESIAN_POINT('Ctrl Pts',(-39.8371685740842,35.4166666666667,23.));
#13850=CARTESIAN_POINT('Ctrl Pts',(-46.,35.2083333333333,12.3256628518317));
#13851=CARTESIAN_POINT('Ctrl Pts',(-46.,35.,0.));
#13852=CARTESIAN_POINT('Ctrl Pts',(-46.,34.7916666666667,-12.3256628518316));
#13853=CARTESIAN_POINT('Ctrl Pts',(-39.8371685740842,34.5833333333333,-23.));
#13854=CARTESIAN_POINT('Ctrl Pts',(-33.6743371481684,34.375,-33.6743371481684));
#13855=CARTESIAN_POINT('Ctrl Pts',(-23.,34.1666666666667,-39.8371685740842));
#13856=CARTESIAN_POINT('Ctrl Pts',(-12.3256628518317,33.9583333333333,-46.));
#13857=CARTESIAN_POINT('Ctrl Pts',(-2.81668763803891E-15,33.75,-46.));
#13858=CARTESIAN_POINT('Ctrl Pts',(12.3256628518316,33.5416666666667,-46.));
#13859=CARTESIAN_POINT('Ctrl Pts',(23.,33.3333333333333,-39.8371685740842));
#13860=CARTESIAN_POINT('Ctrl Pts',(33.6743371481683,33.125,-33.6743371481684));
#13861=CARTESIAN_POINT('Ctrl Pts',(39.8371685740842,32.9166666666667,-23.));
#13862=CARTESIAN_POINT('Ctrl Pts',(46.,32.7083333333333,-12.3256628518317));
#13863=CARTESIAN_POINT('Ctrl Pts',(46.,32.5,-5.63337527607782E-15));
#13864=CARTESIAN_POINT('Ctrl Pts',(46.,32.2916666666667,12.3256628518316));
#13865=CARTESIAN_POINT('Ctrl Pts',(39.8371685740842,32.0833333333333,23.));
#13866=CARTESIAN_POINT('Ctrl Pts',(33.6743371481684,31.875,33.6743371481683));
#13867=CARTESIAN_POINT('Ctrl Pts',(23.,31.6666666666667,39.8371685740842));
#13868=CARTESIAN_POINT('Ctrl Pts',(12.3256628518317,31.4583333333333,46.));
#13869=CARTESIAN_POINT('Ctrl Pts',(8.45006291411674E-15,31.25,46.));
#13870=CARTESIAN_POINT('Ctrl Pts',(-12.3256628518316,31.0416666666667,46.));
#13871=CARTESIAN_POINT('Ctrl Pts',(-23.,30.8333333333333,39.8371685740842));
#13872=CARTESIAN_POINT('Ctrl Pts',(-33.6743371481683,30.625,33.6743371481684));
#13873=CARTESIAN_POINT('Ctrl Pts',(-39.8371685740842,30.4166666666667,23.));
#13874=CARTESIAN_POINT('Ctrl Pts',(-46.,30.2083333333333,12.3256628518317));
#13875=CARTESIAN_POINT('Ctrl Pts',(-46.,30.,0.));
#13876=CARTESIAN_POINT('',(-48.3871149493437,58.4400045958969,-4.33048599679673));
#13877=CARTESIAN_POINT('',(-48.5134353784345,58.3675463684955,-4.33048599679673));
#13878=CARTESIAN_POINT('',(-4.32456003949879,57.3301814056101,-48.3876449370521));
#13879=CARTESIAN_POINT('Ctrl Pts',(-48.3871149493437,58.4400045958969,-4.33048599679673));
#13880=CARTESIAN_POINT('Ctrl Pts',(-47.4315944011671,58.2650323891532,-15.0070896471195));
#13881=CARTESIAN_POINT('Ctrl Pts',(-42.0719562365133,58.0934748917139,-24.2902552584851));
#13882=CARTESIAN_POINT('Ctrl Pts',(-35.5634019560564,57.8851415583806,-35.5634019560564));
#13883=CARTESIAN_POINT('Ctrl Pts',(-24.2902552584851,57.6768082250473,-42.0719562365133));
#13884=CARTESIAN_POINT('Ctrl Pts',(-15.0043879255857,57.5052007984562,-47.4331542408219));
#13885=CARTESIAN_POINT('Ctrl Pts',(-4.32456003949879,57.3301814056101,-48.3876449370521));
#13886=CARTESIAN_POINT('',(-4.32456003949879,57.3301814056101,-48.3876449370521));
#13887=CARTESIAN_POINT('Ctrl Pts',(-48.706329375,58.437500006828,-1.8898197019151E-14));
#13888=CARTESIAN_POINT('Ctrl Pts',(-48.706329375,58.2291666734946,-13.0508216223155));
#13889=CARTESIAN_POINT('Ctrl Pts',(-42.1809185638422,58.0208333401613,-24.3531646875));
#13890=CARTESIAN_POINT('Ctrl Pts',(-35.6555077526845,57.812500006828,-35.6555077526845));
#13891=CARTESIAN_POINT('Ctrl Pts',(-24.3531646875,57.6041666734946,-42.1809185638422));
#13892=CARTESIAN_POINT('Ctrl Pts',(-13.0508216223155,57.3958333401613,-48.706329375));
#13893=CARTESIAN_POINT('Ctrl Pts',(1.59157945007855E-14,57.187500006828,
-48.706329375));
#13894=CARTESIAN_POINT('Ctrl Pts',(13.0508216223155,56.9791666734946,-48.706329375));
#13895=CARTESIAN_POINT('Ctrl Pts',(24.3531646875,56.7708333401613,-42.1809185638422));
#13896=CARTESIAN_POINT('Ctrl Pts',(35.6555077526845,56.562500006828,-35.6555077526845));
#13897=CARTESIAN_POINT('Ctrl Pts',(42.1809185638422,56.3541666734946,-24.3531646875));
#13898=CARTESIAN_POINT('Ctrl Pts',(48.706329375,56.1458333401613,-13.0508216223155));
#13899=CARTESIAN_POINT('Ctrl Pts',(48.706329375,55.937500006828,1.293339198242E-14));
#13900=CARTESIAN_POINT('Ctrl Pts',(48.706329375,55.7291666734946,13.0508216223155));
#13901=CARTESIAN_POINT('Ctrl Pts',(42.1809185638422,55.5208333401613,24.3531646875));
#13902=CARTESIAN_POINT('Ctrl Pts',(35.6555077526845,55.312500006828,35.6555077526845));
#13903=CARTESIAN_POINT('Ctrl Pts',(24.3531646875,55.1041666734946,42.1809185638422));
#13904=CARTESIAN_POINT('Ctrl Pts',(13.0508216223155,54.8958333401613,48.706329375));
#13905=CARTESIAN_POINT('Ctrl Pts',(-9.95098946405443E-15,54.687500006828,
48.706329375));
#13906=CARTESIAN_POINT('Ctrl Pts',(-13.0508216223155,54.4791666734946,48.706329375));
#13907=CARTESIAN_POINT('Ctrl Pts',(-24.3531646875,54.2708333401613,42.1809185638423));
#13908=CARTESIAN_POINT('Ctrl Pts',(-35.6555077526845,54.062500006828,35.6555077526845));
#13909=CARTESIAN_POINT('Ctrl Pts',(-42.1809185638422,53.8541666734946,24.3531646875));
#13910=CARTESIAN_POINT('Ctrl Pts',(-48.706329375,53.6458333401613,13.0508216223155));
#13911=CARTESIAN_POINT('Ctrl Pts',(-48.706329375,53.437500006828,-1.8898197019151E-14));
#13912=CARTESIAN_POINT('Ctrl Pts',(-48.706329375,53.2291666734946,-13.0508216223155));
#13913=CARTESIAN_POINT('Ctrl Pts',(-42.1809185638422,53.0208333401613,-24.3531646875));
#13914=CARTESIAN_POINT('Ctrl Pts',(-35.6555077526845,52.812500006828,-35.6555077526845));
#13915=CARTESIAN_POINT('Ctrl Pts',(-24.3531646875,52.6041666734946,-42.1809185638422));
#13916=CARTESIAN_POINT('Ctrl Pts',(-13.0508216223155,52.3958333401613,-48.706329375));
#13917=CARTESIAN_POINT('Ctrl Pts',(1.59157945007855E-14,52.187500006828,
-48.706329375));
#13918=CARTESIAN_POINT('Ctrl Pts',(13.0508216223155,51.9791666734946,-48.706329375));
#13919=CARTESIAN_POINT('Ctrl Pts',(24.3531646875,51.7708333401613,-42.1809185638422));
#13920=CARTESIAN_POINT('Ctrl Pts',(35.6555077526845,51.562500006828,-35.6555077526845));
#13921=CARTESIAN_POINT('Ctrl Pts',(42.1809185638422,51.3541666734946,-24.3531646875));
#13922=CARTESIAN_POINT('Ctrl Pts',(48.706329375,51.1458333401613,-13.0508216223155));
#13923=CARTESIAN_POINT('Ctrl Pts',(48.706329375,50.937500006828,1.293339198242E-14));
#13924=CARTESIAN_POINT('Ctrl Pts',(48.706329375,50.7291666734946,13.0508216223155));
#13925=CARTESIAN_POINT('Ctrl Pts',(42.1809185638422,50.5208333401613,24.3531646875));
#13926=CARTESIAN_POINT('Ctrl Pts',(35.6555077526845,50.312500006828,35.6555077526845));
#13927=CARTESIAN_POINT('Ctrl Pts',(24.3531646875,50.1041666734946,42.1809185638422));
#13928=CARTESIAN_POINT('Ctrl Pts',(13.0508216223155,49.8958333401613,48.706329375));
#13929=CARTESIAN_POINT('Ctrl Pts',(-9.95098946405443E-15,49.687500006828,
48.706329375));
#13930=CARTESIAN_POINT('Ctrl Pts',(-13.0508216223155,49.4791666734946,48.706329375));
#13931=CARTESIAN_POINT('Ctrl Pts',(-24.3531646875,49.2708333401613,42.1809185638423));
#13932=CARTESIAN_POINT('Ctrl Pts',(-35.6555077526845,49.062500006828,35.6555077526845));
#13933=CARTESIAN_POINT('Ctrl Pts',(-42.1809185638422,48.8541666734946,24.3531646875));
#13934=CARTESIAN_POINT('Ctrl Pts',(-48.706329375,48.6458333401613,13.0508216223155));
#13935=CARTESIAN_POINT('Ctrl Pts',(-48.706329375,48.437500006828,-1.8898197019151E-14));
#13936=CARTESIAN_POINT('Ctrl Pts',(-48.706329375,48.2291666734946,-13.0508216223155));
#13937=CARTESIAN_POINT('Ctrl Pts',(-42.1809185638422,48.0208333401613,-24.3531646875));
#13938=CARTESIAN_POINT('Ctrl Pts',(-35.6555077526845,47.812500006828,-35.6555077526845));
#13939=CARTESIAN_POINT('Ctrl Pts',(-24.3531646875,47.6041666734946,-42.1809185638422));
#13940=CARTESIAN_POINT('Ctrl Pts',(-13.0508216223155,47.3958333401613,-48.706329375));
#13941=CARTESIAN_POINT('Ctrl Pts',(1.59157945007855E-14,47.187500006828,
-48.706329375));
#13942=CARTESIAN_POINT('Ctrl Pts',(13.0508216223155,46.9791666734946,-48.706329375));
#13943=CARTESIAN_POINT('Ctrl Pts',(24.3531646875,46.7708333401613,-42.1809185638422));
#13944=CARTESIAN_POINT('Ctrl Pts',(35.6555077526845,46.562500006828,-35.6555077526845));
#13945=CARTESIAN_POINT('Ctrl Pts',(42.1809185638422,46.3541666734946,-24.3531646875));
#13946=CARTESIAN_POINT('Ctrl Pts',(48.706329375,46.1458333401613,-13.0508216223155));
#13947=CARTESIAN_POINT('Ctrl Pts',(48.706329375,45.937500006828,1.293339198242E-14));
#13948=CARTESIAN_POINT('Ctrl Pts',(48.706329375,45.7291666734946,13.0508216223155));
#13949=CARTESIAN_POINT('Ctrl Pts',(42.1809185638422,45.5208333401613,24.3531646875));
#13950=CARTESIAN_POINT('Ctrl Pts',(35.6555077526845,45.312500006828,35.6555077526845));
#13951=CARTESIAN_POINT('Ctrl Pts',(24.3531646875,45.1041666734946,42.1809185638422));
#13952=CARTESIAN_POINT('Ctrl Pts',(13.0508216223155,44.8958333401613,48.706329375));
#13953=CARTESIAN_POINT('Ctrl Pts',(-9.95098946405443E-15,44.687500006828,
48.706329375));
#13954=CARTESIAN_POINT('Ctrl Pts',(-13.0508216223155,44.4791666734946,48.706329375));
#13955=CARTESIAN_POINT('Ctrl Pts',(-24.3531646875,44.2708333401613,42.1809185638423));
#13956=CARTESIAN_POINT('Ctrl Pts',(-35.6555077526845,44.062500006828,35.6555077526845));
#13957=CARTESIAN_POINT('Ctrl Pts',(-42.1809185638422,43.8541666734946,24.3531646875));
#13958=CARTESIAN_POINT('Ctrl Pts',(-48.706329375,43.6458333401613,13.0508216223155));
#13959=CARTESIAN_POINT('Ctrl Pts',(-48.706329375,43.437500006828,-1.8898197019151E-14));
#13960=CARTESIAN_POINT('Ctrl Pts',(-48.706329375,43.2291666734946,-13.0508216223155));
#13961=CARTESIAN_POINT('Ctrl Pts',(-42.1809185638422,43.0208333401613,-24.3531646875));
#13962=CARTESIAN_POINT('Ctrl Pts',(-35.6555077526845,42.812500006828,-35.6555077526845));
#13963=CARTESIAN_POINT('Ctrl Pts',(-24.3531646875,42.6041666734946,-42.1809185638422));
#13964=CARTESIAN_POINT('Ctrl Pts',(-13.0508216223155,42.3958333401613,-48.706329375));
#13965=CARTESIAN_POINT('Ctrl Pts',(1.59157945007855E-14,42.187500006828,
-48.706329375));
#13966=CARTESIAN_POINT('Ctrl Pts',(13.0508216223155,41.9791666734946,-48.706329375));
#13967=CARTESIAN_POINT('Ctrl Pts',(24.3531646875,41.7708333401613,-42.1809185638422));
#13968=CARTESIAN_POINT('Ctrl Pts',(35.6555077526845,41.562500006828,-35.6555077526845));
#13969=CARTESIAN_POINT('Ctrl Pts',(42.1809185638422,41.3541666734946,-24.3531646875));
#13970=CARTESIAN_POINT('Ctrl Pts',(48.706329375,41.1458333401613,-13.0508216223155));
#13971=CARTESIAN_POINT('Ctrl Pts',(48.706329375,40.937500006828,1.293339198242E-14));
#13972=CARTESIAN_POINT('Ctrl Pts',(48.706329375,40.7291666734946,13.0508216223155));
#13973=CARTESIAN_POINT('Ctrl Pts',(42.1809185638422,40.5208333401613,24.3531646875));
#13974=CARTESIAN_POINT('Ctrl Pts',(35.6555077526845,40.312500006828,35.6555077526845));
#13975=CARTESIAN_POINT('Ctrl Pts',(24.3531646875,40.1041666734946,42.1809185638422));
#13976=CARTESIAN_POINT('Ctrl Pts',(13.0508216223155,39.8958333401613,48.706329375));
#13977=CARTESIAN_POINT('Ctrl Pts',(-9.95098946405443E-15,39.687500006828,
48.706329375));
#13978=CARTESIAN_POINT('Ctrl Pts',(-13.0508216223155,39.4791666734946,48.706329375));
#13979=CARTESIAN_POINT('Ctrl Pts',(-24.3531646875,39.2708333401613,42.1809185638423));
#13980=CARTESIAN_POINT('Ctrl Pts',(-35.6555077526845,39.062500006828,35.6555077526845));
#13981=CARTESIAN_POINT('Ctrl Pts',(-42.1809185638422,38.8541666734946,24.3531646875));
#13982=CARTESIAN_POINT('Ctrl Pts',(-48.706329375,38.6458333401613,13.0508216223155));
#13983=CARTESIAN_POINT('Ctrl Pts',(-48.706329375,38.437500006828,-1.8898197019151E-14));
#13984=CARTESIAN_POINT('Ctrl Pts',(-48.706329375,38.2291666734946,-13.0508216223155));
#13985=CARTESIAN_POINT('Ctrl Pts',(-42.1809185638422,38.0208333401613,-24.3531646875));
#13986=CARTESIAN_POINT('Ctrl Pts',(-35.6555077526845,37.812500006828,-35.6555077526845));
#13987=CARTESIAN_POINT('Ctrl Pts',(-24.3531646875,37.6041666734946,-42.1809185638422));
#13988=CARTESIAN_POINT('Ctrl Pts',(-13.0508216223155,37.3958333401613,-48.706329375));
#13989=CARTESIAN_POINT('Ctrl Pts',(1.59157945007855E-14,37.187500006828,
-48.706329375));
#13990=CARTESIAN_POINT('Ctrl Pts',(13.0508216223155,36.9791666734946,-48.706329375));
#13991=CARTESIAN_POINT('Ctrl Pts',(24.3531646875,36.7708333401613,-42.1809185638422));
#13992=CARTESIAN_POINT('Ctrl Pts',(35.6555077526845,36.562500006828,-35.6555077526845));
#13993=CARTESIAN_POINT('Ctrl Pts',(42.1809185638422,36.3541666734946,-24.3531646875));
#13994=CARTESIAN_POINT('Ctrl Pts',(48.706329375,36.1458333401613,-13.0508216223155));
#13995=CARTESIAN_POINT('Ctrl Pts',(48.706329375,35.937500006828,1.293339198242E-14));
#13996=CARTESIAN_POINT('Ctrl Pts',(48.706329375,35.7291666734946,13.0508216223155));
#13997=CARTESIAN_POINT('Ctrl Pts',(42.1809185638422,35.5208333401613,24.3531646875));
#13998=CARTESIAN_POINT('Ctrl Pts',(35.6555077526845,35.312500006828,35.6555077526845));
#13999=CARTESIAN_POINT('Ctrl Pts',(24.3531646875,35.1041666734946,42.1809185638422));
#14000=CARTESIAN_POINT('Ctrl Pts',(13.0508216223155,34.8958333401613,48.706329375));
#14001=CARTESIAN_POINT('Ctrl Pts',(-9.95098946405443E-15,34.687500006828,
48.706329375));
#14002=CARTESIAN_POINT('Ctrl Pts',(-13.0508216223155,34.4791666734946,48.706329375));
#14003=CARTESIAN_POINT('Ctrl Pts',(-24.3531646875,34.2708333401613,42.1809185638423));
#14004=CARTESIAN_POINT('Ctrl Pts',(-35.6555077526845,34.062500006828,35.6555077526845));
#14005=CARTESIAN_POINT('Ctrl Pts',(-42.1809185638422,33.8541666734946,24.3531646875));
#14006=CARTESIAN_POINT('Ctrl Pts',(-48.706329375,33.6458333401613,13.0508216223155));
#14007=CARTESIAN_POINT('Ctrl Pts',(-48.706329375,33.437500006828,-1.8898197019151E-14));
#14008=CARTESIAN_POINT('Ctrl Pts',(-48.706329375,33.2291666734946,-13.0508216223155));
#14009=CARTESIAN_POINT('Ctrl Pts',(-42.1809185638422,33.0208333401613,-24.3531646875));
#14010=CARTESIAN_POINT('Ctrl Pts',(-35.6555077526845,32.812500006828,-35.6555077526845));
#14011=CARTESIAN_POINT('Ctrl Pts',(-24.3531646875,32.6041666734946,-42.1809185638422));
#14012=CARTESIAN_POINT('Ctrl Pts',(-13.0508216223155,32.3958333401613,-48.706329375));
#14013=CARTESIAN_POINT('Ctrl Pts',(1.59157945007855E-14,32.187500006828,
-48.706329375));
#14014=CARTESIAN_POINT('Ctrl Pts',(13.0508216223155,31.9791666734946,-48.706329375));
#14015=CARTESIAN_POINT('Ctrl Pts',(24.3531646875,31.7708333401613,-42.1809185638422));
#14016=CARTESIAN_POINT('Ctrl Pts',(35.6555077526845,31.562500006828,-35.6555077526845));
#14017=CARTESIAN_POINT('Ctrl Pts',(42.1809185638422,31.3541666734946,-24.3531646875));
#14018=CARTESIAN_POINT('Ctrl Pts',(48.706329375,31.1458333401613,-13.0508216223155));
#14019=CARTESIAN_POINT('Ctrl Pts',(48.706329375,30.937500006828,1.293339198242E-14));
#14020=CARTESIAN_POINT('Ctrl Pts',(48.706329375,30.7291666734946,13.0508216223155));
#14021=CARTESIAN_POINT('Ctrl Pts',(42.1809185638422,30.5208333401613,24.3531646875));
#14022=CARTESIAN_POINT('Ctrl Pts',(35.6555077526845,30.312500006828,35.6555077526845));
#14023=CARTESIAN_POINT('Ctrl Pts',(24.3531646875,30.1041666734946,42.1809185638422));
#14024=CARTESIAN_POINT('Ctrl Pts',(13.0508216223155,29.8958333401613,48.706329375));
#14025=CARTESIAN_POINT('Ctrl Pts',(-9.95098946405443E-15,29.687500006828,
48.706329375));
#14026=CARTESIAN_POINT('Ctrl Pts',(-13.0508216223155,29.4791666734946,48.706329375));
#14027=CARTESIAN_POINT('Ctrl Pts',(-24.3531646875,29.2708333401613,42.1809185638423));
#14028=CARTESIAN_POINT('Ctrl Pts',(-35.6555077526845,29.062500006828,35.6555077526845));
#14029=CARTESIAN_POINT('Ctrl Pts',(-42.1809185638422,28.8541666734946,24.3531646875));
#14030=CARTESIAN_POINT('Ctrl Pts',(-48.706329375,28.6458333401613,13.0508216223155));
#14031=CARTESIAN_POINT('Ctrl Pts',(-48.706329375,28.437500006828,-1.8898197019151E-14));
#14032=CARTESIAN_POINT('Ctrl Pts',(-46.,60.,0.));
#14033=CARTESIAN_POINT('Ctrl Pts',(-46.,59.7916666666667,-12.3256628518316));
#14034=CARTESIAN_POINT('Ctrl Pts',(-39.8371685740842,59.5833333333333,-23.));
#14035=CARTESIAN_POINT('Ctrl Pts',(-33.6743371481684,59.375,-33.6743371481684));
#14036=CARTESIAN_POINT('Ctrl Pts',(-23.,59.1666666666667,-39.8371685740842));
#14037=CARTESIAN_POINT('Ctrl Pts',(-12.3256628518317,58.9583333333333,-46.));
#14038=CARTESIAN_POINT('Ctrl Pts',(-2.81668763803891E-15,58.75,-46.));
#14039=CARTESIAN_POINT('Ctrl Pts',(12.3256628518316,58.5416666666667,-46.));
#14040=CARTESIAN_POINT('Ctrl Pts',(23.,58.3333333333333,-39.8371685740842));
#14041=CARTESIAN_POINT('Ctrl Pts',(33.6743371481683,58.125,-33.6743371481684));
#14042=CARTESIAN_POINT('Ctrl Pts',(39.8371685740842,57.9166666666667,-23.));
#14043=CARTESIAN_POINT('Ctrl Pts',(46.,57.7083333333333,-12.3256628518317));
#14044=CARTESIAN_POINT('Ctrl Pts',(46.,57.5,-5.63337527607782E-15));
#14045=CARTESIAN_POINT('Ctrl Pts',(46.,57.2916666666667,12.3256628518316));
#14046=CARTESIAN_POINT('Ctrl Pts',(39.8371685740842,57.0833333333333,23.));
#14047=CARTESIAN_POINT('Ctrl Pts',(33.6743371481684,56.875,33.6743371481683));
#14048=CARTESIAN_POINT('Ctrl Pts',(23.,56.6666666666667,39.8371685740842));
#14049=CARTESIAN_POINT('Ctrl Pts',(12.3256628518317,56.4583333333333,46.));
#14050=CARTESIAN_POINT('Ctrl Pts',(8.45006291411674E-15,56.25,46.));
#14051=CARTESIAN_POINT('Ctrl Pts',(-12.3256628518316,56.0416666666667,46.));
#14052=CARTESIAN_POINT('Ctrl Pts',(-23.,55.8333333333333,39.8371685740842));
#14053=CARTESIAN_POINT('Ctrl Pts',(-33.6743371481683,55.625,33.6743371481684));
#14054=CARTESIAN_POINT('Ctrl Pts',(-39.8371685740842,55.4166666666667,23.));
#14055=CARTESIAN_POINT('Ctrl Pts',(-46.,55.2083333333333,12.3256628518317));
#14056=CARTESIAN_POINT('Ctrl Pts',(-46.,55.,0.));
#14057=CARTESIAN_POINT('Ctrl Pts',(-46.,54.7916666666667,-12.3256628518316));
#14058=CARTESIAN_POINT('Ctrl Pts',(-39.8371685740842,54.5833333333333,-23.));
#14059=CARTESIAN_POINT('Ctrl Pts',(-33.6743371481684,54.375,-33.6743371481684));
#14060=CARTESIAN_POINT('Ctrl Pts',(-23.,54.1666666666667,-39.8371685740842));
#14061=CARTESIAN_POINT('Ctrl Pts',(-12.3256628518317,53.9583333333333,-46.));
#14062=CARTESIAN_POINT('Ctrl Pts',(-2.81668763803891E-15,53.75,-46.));
#14063=CARTESIAN_POINT('Ctrl Pts',(12.3256628518316,53.5416666666667,-46.));
#14064=CARTESIAN_POINT('Ctrl Pts',(23.,53.3333333333333,-39.8371685740842));
#14065=CARTESIAN_POINT('Ctrl Pts',(33.6743371481683,53.125,-33.6743371481684));
#14066=CARTESIAN_POINT('Ctrl Pts',(39.8371685740842,52.9166666666667,-23.));
#14067=CARTESIAN_POINT('Ctrl Pts',(46.,52.7083333333333,-12.3256628518317));
#14068=CARTESIAN_POINT('Ctrl Pts',(46.,52.5,-5.63337527607782E-15));
#14069=CARTESIAN_POINT('Ctrl Pts',(46.,52.2916666666667,12.3256628518316));
#14070=CARTESIAN_POINT('Ctrl Pts',(39.8371685740842,52.0833333333333,23.));
#14071=CARTESIAN_POINT('Ctrl Pts',(33.6743371481684,51.875,33.6743371481683));
#14072=CARTESIAN_POINT('Ctrl Pts',(23.,51.6666666666667,39.8371685740842));
#14073=CARTESIAN_POINT('Ctrl Pts',(12.3256628518317,51.4583333333333,46.));
#14074=CARTESIAN_POINT('Ctrl Pts',(8.45006291411674E-15,51.25,46.));
#14075=CARTESIAN_POINT('Ctrl Pts',(-12.3256628518316,51.0416666666667,46.));
#14076=CARTESIAN_POINT('Ctrl Pts',(-23.,50.8333333333333,39.8371685740842));
#14077=CARTESIAN_POINT('Ctrl Pts',(-33.6743371481683,50.625,33.6743371481684));
#14078=CARTESIAN_POINT('Ctrl Pts',(-39.8371685740842,50.4166666666667,23.));
#14079=CARTESIAN_POINT('Ctrl Pts',(-46.,50.2083333333333,12.3256628518317));
#14080=CARTESIAN_POINT('Ctrl Pts',(-46.,50.,0.));
#14081=CARTESIAN_POINT('Ctrl Pts',(-46.,49.7916666666667,-12.3256628518316));
#14082=CARTESIAN_POINT('Ctrl Pts',(-39.8371685740842,49.5833333333333,-23.));
#14083=CARTESIAN_POINT('Ctrl Pts',(-33.6743371481684,49.375,-33.6743371481684));
#14084=CARTESIAN_POINT('Ctrl Pts',(-23.,49.1666666666667,-39.8371685740842));
#14085=CARTESIAN_POINT('Ctrl Pts',(-12.3256628518317,48.9583333333333,-46.));
#14086=CARTESIAN_POINT('Ctrl Pts',(-2.81668763803891E-15,48.75,-46.));
#14087=CARTESIAN_POINT('Ctrl Pts',(12.3256628518316,48.5416666666667,-46.));
#14088=CARTESIAN_POINT('Ctrl Pts',(23.,48.3333333333333,-39.8371685740842));
#14089=CARTESIAN_POINT('Ctrl Pts',(33.6743371481683,48.125,-33.6743371481684));
#14090=CARTESIAN_POINT('Ctrl Pts',(39.8371685740842,47.9166666666667,-23.));
#14091=CARTESIAN_POINT('Ctrl Pts',(46.,47.7083333333333,-12.3256628518317));
#14092=CARTESIAN_POINT('Ctrl Pts',(46.,47.5,-5.63337527607782E-15));
#14093=CARTESIAN_POINT('Ctrl Pts',(46.,47.2916666666667,12.3256628518316));
#14094=CARTESIAN_POINT('Ctrl Pts',(39.8371685740842,47.0833333333333,23.));
#14095=CARTESIAN_POINT('Ctrl Pts',(33.6743371481684,46.875,33.6743371481683));
#14096=CARTESIAN_POINT('Ctrl Pts',(23.,46.6666666666667,39.8371685740842));
#14097=CARTESIAN_POINT('Ctrl Pts',(12.3256628518317,46.4583333333333,46.));
#14098=CARTESIAN_POINT('Ctrl Pts',(8.45006291411674E-15,46.25,46.));
#14099=CARTESIAN_POINT('Ctrl Pts',(-12.3256628518316,46.0416666666667,46.));
#14100=CARTESIAN_POINT('Ctrl Pts',(-23.,45.8333333333333,39.8371685740842));
#14101=CARTESIAN_POINT('Ctrl Pts',(-33.6743371481683,45.625,33.6743371481684));
#14102=CARTESIAN_POINT('Ctrl Pts',(-39.8371685740842,45.4166666666667,23.));
#14103=CARTESIAN_POINT('Ctrl Pts',(-46.,45.2083333333333,12.3256628518317));
#14104=CARTESIAN_POINT('Ctrl Pts',(-46.,45.,0.));
#14105=CARTESIAN_POINT('Ctrl Pts',(-46.,44.7916666666667,-12.3256628518316));
#14106=CARTESIAN_POINT('Ctrl Pts',(-39.8371685740842,44.5833333333333,-23.));
#14107=CARTESIAN_POINT('Ctrl Pts',(-33.6743371481684,44.375,-33.6743371481684));
#14108=CARTESIAN_POINT('Ctrl Pts',(-23.,44.1666666666667,-39.8371685740842));
#14109=CARTESIAN_POINT('Ctrl Pts',(-12.3256628518317,43.9583333333333,-46.));
#14110=CARTESIAN_POINT('Ctrl Pts',(-2.81668763803891E-15,43.75,-46.));
#14111=CARTESIAN_POINT('Ctrl Pts',(12.3256628518316,43.5416666666667,-46.));
#14112=CARTESIAN_POINT('Ctrl Pts',(23.,43.3333333333333,-39.8371685740842));
#14113=CARTESIAN_POINT('Ctrl Pts',(33.6743371481683,43.125,-33.6743371481684));
#14114=CARTESIAN_POINT('Ctrl Pts',(39.8371685740842,42.9166666666667,-23.));
#14115=CARTESIAN_POINT('Ctrl Pts',(46.,42.7083333333333,-12.3256628518317));
#14116=CARTESIAN_POINT('Ctrl Pts',(46.,42.5,-5.63337527607782E-15));
#14117=CARTESIAN_POINT('Ctrl Pts',(46.,42.2916666666667,12.3256628518316));
#14118=CARTESIAN_POINT('Ctrl Pts',(39.8371685740842,42.0833333333333,23.));
#14119=CARTESIAN_POINT('Ctrl Pts',(33.6743371481684,41.875,33.6743371481683));
#14120=CARTESIAN_POINT('Ctrl Pts',(23.,41.6666666666667,39.8371685740842));
#14121=CARTESIAN_POINT('Ctrl Pts',(12.3256628518317,41.4583333333333,46.));
#14122=CARTESIAN_POINT('Ctrl Pts',(8.45006291411674E-15,41.25,46.));
#14123=CARTESIAN_POINT('Ctrl Pts',(-12.3256628518316,41.0416666666667,46.));
#14124=CARTESIAN_POINT('Ctrl Pts',(-23.,40.8333333333333,39.8371685740842));
#14125=CARTESIAN_POINT('Ctrl Pts',(-33.6743371481683,40.625,33.6743371481684));
#14126=CARTESIAN_POINT('Ctrl Pts',(-39.8371685740842,40.4166666666667,23.));
#14127=CARTESIAN_POINT('Ctrl Pts',(-46.,40.2083333333333,12.3256628518317));
#14128=CARTESIAN_POINT('Ctrl Pts',(-46.,40.,0.));
#14129=CARTESIAN_POINT('Ctrl Pts',(-46.,39.7916666666667,-12.3256628518316));
#14130=CARTESIAN_POINT('Ctrl Pts',(-39.8371685740842,39.5833333333333,-23.));
#14131=CARTESIAN_POINT('Ctrl Pts',(-33.6743371481684,39.375,-33.6743371481684));
#14132=CARTESIAN_POINT('Ctrl Pts',(-23.,39.1666666666667,-39.8371685740842));
#14133=CARTESIAN_POINT('Ctrl Pts',(-12.3256628518317,38.9583333333333,-46.));
#14134=CARTESIAN_POINT('Ctrl Pts',(-2.81668763803891E-15,38.75,-46.));
#14135=CARTESIAN_POINT('Ctrl Pts',(12.3256628518316,38.5416666666667,-46.));
#14136=CARTESIAN_POINT('Ctrl Pts',(23.,38.3333333333333,-39.8371685740842));
#14137=CARTESIAN_POINT('Ctrl Pts',(33.6743371481683,38.125,-33.6743371481684));
#14138=CARTESIAN_POINT('Ctrl Pts',(39.8371685740842,37.9166666666667,-23.));
#14139=CARTESIAN_POINT('Ctrl Pts',(46.,37.7083333333333,-12.3256628518317));
#14140=CARTESIAN_POINT('Ctrl Pts',(46.,37.5,-5.63337527607782E-15));
#14141=CARTESIAN_POINT('Ctrl Pts',(46.,37.2916666666667,12.3256628518316));
#14142=CARTESIAN_POINT('Ctrl Pts',(39.8371685740842,37.0833333333333,23.));
#14143=CARTESIAN_POINT('Ctrl Pts',(33.6743371481684,36.875,33.6743371481683));
#14144=CARTESIAN_POINT('Ctrl Pts',(23.,36.6666666666667,39.8371685740842));
#14145=CARTESIAN_POINT('Ctrl Pts',(12.3256628518317,36.4583333333333,46.));
#14146=CARTESIAN_POINT('Ctrl Pts',(8.45006291411674E-15,36.25,46.));
#14147=CARTESIAN_POINT('Ctrl Pts',(-12.3256628518316,36.0416666666667,46.));
#14148=CARTESIAN_POINT('Ctrl Pts',(-23.,35.8333333333333,39.8371685740842));
#14149=CARTESIAN_POINT('Ctrl Pts',(-33.6743371481683,35.625,33.6743371481684));
#14150=CARTESIAN_POINT('Ctrl Pts',(-39.8371685740842,35.4166666666667,23.));
#14151=CARTESIAN_POINT('Ctrl Pts',(-46.,35.2083333333333,12.3256628518317));
#14152=CARTESIAN_POINT('Ctrl Pts',(-46.,35.,0.));
#14153=CARTESIAN_POINT('Ctrl Pts',(-46.,34.7916666666667,-12.3256628518316));
#14154=CARTESIAN_POINT('Ctrl Pts',(-39.8371685740842,34.5833333333333,-23.));
#14155=CARTESIAN_POINT('Ctrl Pts',(-33.6743371481684,34.375,-33.6743371481684));
#14156=CARTESIAN_POINT('Ctrl Pts',(-23.,34.1666666666667,-39.8371685740842));
#14157=CARTESIAN_POINT('Ctrl Pts',(-12.3256628518317,33.9583333333333,-46.));
#14158=CARTESIAN_POINT('Ctrl Pts',(-2.81668763803891E-15,33.75,-46.));
#14159=CARTESIAN_POINT('Ctrl Pts',(12.3256628518316,33.5416666666667,-46.));
#14160=CARTESIAN_POINT('Ctrl Pts',(23.,33.3333333333333,-39.8371685740842));
#14161=CARTESIAN_POINT('Ctrl Pts',(33.6743371481683,33.125,-33.6743371481684));
#14162=CARTESIAN_POINT('Ctrl Pts',(39.8371685740842,32.9166666666667,-23.));
#14163=CARTESIAN_POINT('Ctrl Pts',(46.,32.7083333333333,-12.3256628518317));
#14164=CARTESIAN_POINT('Ctrl Pts',(46.,32.5,-5.63337527607782E-15));
#14165=CARTESIAN_POINT('Ctrl Pts',(46.,32.2916666666667,12.3256628518316));
#14166=CARTESIAN_POINT('Ctrl Pts',(39.8371685740842,32.0833333333333,23.));
#14167=CARTESIAN_POINT('Ctrl Pts',(33.6743371481684,31.875,33.6743371481683));
#14168=CARTESIAN_POINT('Ctrl Pts',(23.,31.6666666666667,39.8371685740842));
#14169=CARTESIAN_POINT('Ctrl Pts',(12.3256628518317,31.4583333333333,46.));
#14170=CARTESIAN_POINT('Ctrl Pts',(8.45006291411674E-15,31.25,46.));
#14171=CARTESIAN_POINT('Ctrl Pts',(-12.3256628518316,31.0416666666667,46.));
#14172=CARTESIAN_POINT('Ctrl Pts',(-23.,30.8333333333333,39.8371685740842));
#14173=CARTESIAN_POINT('Ctrl Pts',(-33.6743371481683,30.625,33.6743371481684));
#14174=CARTESIAN_POINT('Ctrl Pts',(-39.8371685740842,30.4166666666667,23.));
#14175=CARTESIAN_POINT('Ctrl Pts',(-46.,30.2083333333333,12.3256628518317));
#14176=CARTESIAN_POINT('Ctrl Pts',(-46.,30.,0.));
#14177=CARTESIAN_POINT('Origin',(4513.80899678944,-7900.15854878091,-4.33048595875475));
#14178=CARTESIAN_POINT('Ctrl Pts',(-4.32456003949879,53.8240181593938,-45.7962681936506));
#14179=CARTESIAN_POINT('Ctrl Pts',(-4.32456003949879,53.6905125468623,-46.0278818021281));
#14180=CARTESIAN_POINT('Ctrl Pts',(-4.32456003949875,53.4234964717135,-46.4911062234486));
#14181=CARTESIAN_POINT('Ctrl Pts',(-4.32456003949878,53.1564711191154,-46.954325296818));
#14182=CARTESIAN_POINT('Ctrl Pts',(-4.32456003949878,52.7677643029224,-47.6286149142205));
#14183=CARTESIAN_POINT('Ctrl Pts',(-4.32456003949881,52.5125642776457,-48.0712916022845));
#14184=CARTESIAN_POINT('Ctrl Pts',(-4.32456003949876,52.2573567866782,-48.5139639861634));
#14185=CARTESIAN_POINT('Ctrl Pts',(-48.706329375,58.437500006828,-1.8898197019151E-14));
#14186=CARTESIAN_POINT('Ctrl Pts',(-48.706329375,58.2291666734946,-13.0508216223155));
#14187=CARTESIAN_POINT('Ctrl Pts',(-42.1809185638422,58.0208333401613,-24.3531646875));
#14188=CARTESIAN_POINT('Ctrl Pts',(-35.6555077526845,57.812500006828,-35.6555077526845));
#14189=CARTESIAN_POINT('Ctrl Pts',(-24.3531646875,57.6041666734946,-42.1809185638422));
#14190=CARTESIAN_POINT('Ctrl Pts',(-13.0508216223155,57.3958333401613,-48.706329375));
#14191=CARTESIAN_POINT('Ctrl Pts',(1.59157945007855E-14,57.187500006828,
-48.706329375));
#14192=CARTESIAN_POINT('Ctrl Pts',(13.0508216223155,56.9791666734946,-48.706329375));
#14193=CARTESIAN_POINT('Ctrl Pts',(24.3531646875,56.7708333401613,-42.1809185638422));
#14194=CARTESIAN_POINT('Ctrl Pts',(35.6555077526845,56.562500006828,-35.6555077526845));
#14195=CARTESIAN_POINT('Ctrl Pts',(42.1809185638422,56.3541666734946,-24.3531646875));
#14196=CARTESIAN_POINT('Ctrl Pts',(48.706329375,56.1458333401613,-13.0508216223155));
#14197=CARTESIAN_POINT('Ctrl Pts',(48.706329375,55.937500006828,1.293339198242E-14));
#14198=CARTESIAN_POINT('Ctrl Pts',(48.706329375,55.7291666734946,13.0508216223155));
#14199=CARTESIAN_POINT('Ctrl Pts',(42.1809185638422,55.5208333401613,24.3531646875));
#14200=CARTESIAN_POINT('Ctrl Pts',(35.6555077526845,55.312500006828,35.6555077526845));
#14201=CARTESIAN_POINT('Ctrl Pts',(24.3531646875,55.1041666734946,42.1809185638422));
#14202=CARTESIAN_POINT('Ctrl Pts',(13.0508216223155,54.8958333401613,48.706329375));
#14203=CARTESIAN_POINT('Ctrl Pts',(-9.95098946405443E-15,54.687500006828,
48.706329375));
#14204=CARTESIAN_POINT('Ctrl Pts',(-13.0508216223155,54.4791666734946,48.706329375));
#14205=CARTESIAN_POINT('Ctrl Pts',(-24.3531646875,54.2708333401613,42.1809185638423));
#14206=CARTESIAN_POINT('Ctrl Pts',(-35.6555077526845,54.062500006828,35.6555077526845));
#14207=CARTESIAN_POINT('Ctrl Pts',(-42.1809185638422,53.8541666734946,24.3531646875));
#14208=CARTESIAN_POINT('Ctrl Pts',(-48.706329375,53.6458333401613,13.0508216223155));
#14209=CARTESIAN_POINT('Ctrl Pts',(-48.706329375,53.437500006828,-1.8898197019151E-14));
#14210=CARTESIAN_POINT('Ctrl Pts',(-48.706329375,53.2291666734946,-13.0508216223155));
#14211=CARTESIAN_POINT('Ctrl Pts',(-42.1809185638422,53.0208333401613,-24.3531646875));
#14212=CARTESIAN_POINT('Ctrl Pts',(-35.6555077526845,52.812500006828,-35.6555077526845));
#14213=CARTESIAN_POINT('Ctrl Pts',(-24.3531646875,52.6041666734946,-42.1809185638422));
#14214=CARTESIAN_POINT('Ctrl Pts',(-13.0508216223155,52.3958333401613,-48.706329375));
#14215=CARTESIAN_POINT('Ctrl Pts',(1.59157945007855E-14,52.187500006828,
-48.706329375));
#14216=CARTESIAN_POINT('Ctrl Pts',(13.0508216223155,51.9791666734946,-48.706329375));
#14217=CARTESIAN_POINT('Ctrl Pts',(24.3531646875,51.7708333401613,-42.1809185638422));
#14218=CARTESIAN_POINT('Ctrl Pts',(35.6555077526845,51.562500006828,-35.6555077526845));
#14219=CARTESIAN_POINT('Ctrl Pts',(42.1809185638422,51.3541666734946,-24.3531646875));
#14220=CARTESIAN_POINT('Ctrl Pts',(48.706329375,51.1458333401613,-13.0508216223155));
#14221=CARTESIAN_POINT('Ctrl Pts',(48.706329375,50.937500006828,1.293339198242E-14));
#14222=CARTESIAN_POINT('Ctrl Pts',(48.706329375,50.7291666734946,13.0508216223155));
#14223=CARTESIAN_POINT('Ctrl Pts',(42.1809185638422,50.5208333401613,24.3531646875));
#14224=CARTESIAN_POINT('Ctrl Pts',(35.6555077526845,50.312500006828,35.6555077526845));
#14225=CARTESIAN_POINT('Ctrl Pts',(24.3531646875,50.1041666734946,42.1809185638422));
#14226=CARTESIAN_POINT('Ctrl Pts',(13.0508216223155,49.8958333401613,48.706329375));
#14227=CARTESIAN_POINT('Ctrl Pts',(-9.95098946405443E-15,49.687500006828,
48.706329375));
#14228=CARTESIAN_POINT('Ctrl Pts',(-13.0508216223155,49.4791666734946,48.706329375));
#14229=CARTESIAN_POINT('Ctrl Pts',(-24.3531646875,49.2708333401613,42.1809185638423));
#14230=CARTESIAN_POINT('Ctrl Pts',(-35.6555077526845,49.062500006828,35.6555077526845));
#14231=CARTESIAN_POINT('Ctrl Pts',(-42.1809185638422,48.8541666734946,24.3531646875));
#14232=CARTESIAN_POINT('Ctrl Pts',(-48.706329375,48.6458333401613,13.0508216223155));
#14233=CARTESIAN_POINT('Ctrl Pts',(-48.706329375,48.437500006828,-1.8898197019151E-14));
#14234=CARTESIAN_POINT('Ctrl Pts',(-48.706329375,48.2291666734946,-13.0508216223155));
#14235=CARTESIAN_POINT('Ctrl Pts',(-42.1809185638422,48.0208333401613,-24.3531646875));
#14236=CARTESIAN_POINT('Ctrl Pts',(-35.6555077526845,47.812500006828,-35.6555077526845));
#14237=CARTESIAN_POINT('Ctrl Pts',(-24.3531646875,47.6041666734946,-42.1809185638422));
#14238=CARTESIAN_POINT('Ctrl Pts',(-13.0508216223155,47.3958333401613,-48.706329375));
#14239=CARTESIAN_POINT('Ctrl Pts',(1.59157945007855E-14,47.187500006828,
-48.706329375));
#14240=CARTESIAN_POINT('Ctrl Pts',(13.0508216223155,46.9791666734946,-48.706329375));
#14241=CARTESIAN_POINT('Ctrl Pts',(24.3531646875,46.7708333401613,-42.1809185638422));
#14242=CARTESIAN_POINT('Ctrl Pts',(35.6555077526845,46.562500006828,-35.6555077526845));
#14243=CARTESIAN_POINT('Ctrl Pts',(42.1809185638422,46.3541666734946,-24.3531646875));
#14244=CARTESIAN_POINT('Ctrl Pts',(48.706329375,46.1458333401613,-13.0508216223155));
#14245=CARTESIAN_POINT('Ctrl Pts',(48.706329375,45.937500006828,1.293339198242E-14));
#14246=CARTESIAN_POINT('Ctrl Pts',(48.706329375,45.7291666734946,13.0508216223155));
#14247=CARTESIAN_POINT('Ctrl Pts',(42.1809185638422,45.5208333401613,24.3531646875));
#14248=CARTESIAN_POINT('Ctrl Pts',(35.6555077526845,45.312500006828,35.6555077526845));
#14249=CARTESIAN_POINT('Ctrl Pts',(24.3531646875,45.1041666734946,42.1809185638422));
#14250=CARTESIAN_POINT('Ctrl Pts',(13.0508216223155,44.8958333401613,48.706329375));
#14251=CARTESIAN_POINT('Ctrl Pts',(-9.95098946405443E-15,44.687500006828,
48.706329375));
#14252=CARTESIAN_POINT('Ctrl Pts',(-13.0508216223155,44.4791666734946,48.706329375));
#14253=CARTESIAN_POINT('Ctrl Pts',(-24.3531646875,44.2708333401613,42.1809185638423));
#14254=CARTESIAN_POINT('Ctrl Pts',(-35.6555077526845,44.062500006828,35.6555077526845));
#14255=CARTESIAN_POINT('Ctrl Pts',(-42.1809185638422,43.8541666734946,24.3531646875));
#14256=CARTESIAN_POINT('Ctrl Pts',(-48.706329375,43.6458333401613,13.0508216223155));
#14257=CARTESIAN_POINT('Ctrl Pts',(-48.706329375,43.437500006828,-1.8898197019151E-14));
#14258=CARTESIAN_POINT('Ctrl Pts',(-48.706329375,43.2291666734946,-13.0508216223155));
#14259=CARTESIAN_POINT('Ctrl Pts',(-42.1809185638422,43.0208333401613,-24.3531646875));
#14260=CARTESIAN_POINT('Ctrl Pts',(-35.6555077526845,42.812500006828,-35.6555077526845));
#14261=CARTESIAN_POINT('Ctrl Pts',(-24.3531646875,42.6041666734946,-42.1809185638422));
#14262=CARTESIAN_POINT('Ctrl Pts',(-13.0508216223155,42.3958333401613,-48.706329375));
#14263=CARTESIAN_POINT('Ctrl Pts',(1.59157945007855E-14,42.187500006828,
-48.706329375));
#14264=CARTESIAN_POINT('Ctrl Pts',(13.0508216223155,41.9791666734946,-48.706329375));
#14265=CARTESIAN_POINT('Ctrl Pts',(24.3531646875,41.7708333401613,-42.1809185638422));
#14266=CARTESIAN_POINT('Ctrl Pts',(35.6555077526845,41.562500006828,-35.6555077526845));
#14267=CARTESIAN_POINT('Ctrl Pts',(42.1809185638422,41.3541666734946,-24.3531646875));
#14268=CARTESIAN_POINT('Ctrl Pts',(48.706329375,41.1458333401613,-13.0508216223155));
#14269=CARTESIAN_POINT('Ctrl Pts',(48.706329375,40.937500006828,1.293339198242E-14));
#14270=CARTESIAN_POINT('Ctrl Pts',(48.706329375,40.7291666734946,13.0508216223155));
#14271=CARTESIAN_POINT('Ctrl Pts',(42.1809185638422,40.5208333401613,24.3531646875));
#14272=CARTESIAN_POINT('Ctrl Pts',(35.6555077526845,40.312500006828,35.6555077526845));
#14273=CARTESIAN_POINT('Ctrl Pts',(24.3531646875,40.1041666734946,42.1809185638422));
#14274=CARTESIAN_POINT('Ctrl Pts',(13.0508216223155,39.8958333401613,48.706329375));
#14275=CARTESIAN_POINT('Ctrl Pts',(-9.95098946405443E-15,39.687500006828,
48.706329375));
#14276=CARTESIAN_POINT('Ctrl Pts',(-13.0508216223155,39.4791666734946,48.706329375));
#14277=CARTESIAN_POINT('Ctrl Pts',(-24.3531646875,39.2708333401613,42.1809185638423));
#14278=CARTESIAN_POINT('Ctrl Pts',(-35.6555077526845,39.062500006828,35.6555077526845));
#14279=CARTESIAN_POINT('Ctrl Pts',(-42.1809185638422,38.8541666734946,24.3531646875));
#14280=CARTESIAN_POINT('Ctrl Pts',(-48.706329375,38.6458333401613,13.0508216223155));
#14281=CARTESIAN_POINT('Ctrl Pts',(-48.706329375,38.437500006828,-1.8898197019151E-14));
#14282=CARTESIAN_POINT('Ctrl Pts',(-48.706329375,38.2291666734946,-13.0508216223155));
#14283=CARTESIAN_POINT('Ctrl Pts',(-42.1809185638422,38.0208333401613,-24.3531646875));
#14284=CARTESIAN_POINT('Ctrl Pts',(-35.6555077526845,37.812500006828,-35.6555077526845));
#14285=CARTESIAN_POINT('Ctrl Pts',(-24.3531646875,37.6041666734946,-42.1809185638422));
#14286=CARTESIAN_POINT('Ctrl Pts',(-13.0508216223155,37.3958333401613,-48.706329375));
#14287=CARTESIAN_POINT('Ctrl Pts',(1.59157945007855E-14,37.187500006828,
-48.706329375));
#14288=CARTESIAN_POINT('Ctrl Pts',(13.0508216223155,36.9791666734946,-48.706329375));
#14289=CARTESIAN_POINT('Ctrl Pts',(24.3531646875,36.7708333401613,-42.1809185638422));
#14290=CARTESIAN_POINT('Ctrl Pts',(35.6555077526845,36.562500006828,-35.6555077526845));
#14291=CARTESIAN_POINT('Ctrl Pts',(42.1809185638422,36.3541666734946,-24.3531646875));
#14292=CARTESIAN_POINT('Ctrl Pts',(48.706329375,36.1458333401613,-13.0508216223155));
#14293=CARTESIAN_POINT('Ctrl Pts',(48.706329375,35.937500006828,1.293339198242E-14));
#14294=CARTESIAN_POINT('Ctrl Pts',(48.706329375,35.7291666734946,13.0508216223155));
#14295=CARTESIAN_POINT('Ctrl Pts',(42.1809185638422,35.5208333401613,24.3531646875));
#14296=CARTESIAN_POINT('Ctrl Pts',(35.6555077526845,35.312500006828,35.6555077526845));
#14297=CARTESIAN_POINT('Ctrl Pts',(24.3531646875,35.1041666734946,42.1809185638422));
#14298=CARTESIAN_POINT('Ctrl Pts',(13.0508216223155,34.8958333401613,48.706329375));
#14299=CARTESIAN_POINT('Ctrl Pts',(-9.95098946405443E-15,34.687500006828,
48.706329375));
#14300=CARTESIAN_POINT('Ctrl Pts',(-13.0508216223155,34.4791666734946,48.706329375));
#14301=CARTESIAN_POINT('Ctrl Pts',(-24.3531646875,34.2708333401613,42.1809185638423));
#14302=CARTESIAN_POINT('Ctrl Pts',(-35.6555077526845,34.062500006828,35.6555077526845));
#14303=CARTESIAN_POINT('Ctrl Pts',(-42.1809185638422,33.8541666734946,24.3531646875));
#14304=CARTESIAN_POINT('Ctrl Pts',(-48.706329375,33.6458333401613,13.0508216223155));
#14305=CARTESIAN_POINT('Ctrl Pts',(-48.706329375,33.437500006828,-1.8898197019151E-14));
#14306=CARTESIAN_POINT('Ctrl Pts',(-48.706329375,33.2291666734946,-13.0508216223155));
#14307=CARTESIAN_POINT('Ctrl Pts',(-42.1809185638422,33.0208333401613,-24.3531646875));
#14308=CARTESIAN_POINT('Ctrl Pts',(-35.6555077526845,32.812500006828,-35.6555077526845));
#14309=CARTESIAN_POINT('Ctrl Pts',(-24.3531646875,32.6041666734946,-42.1809185638422));
#14310=CARTESIAN_POINT('Ctrl Pts',(-13.0508216223155,32.3958333401613,-48.706329375));
#14311=CARTESIAN_POINT('Ctrl Pts',(1.59157945007855E-14,32.187500006828,
-48.706329375));
#14312=CARTESIAN_POINT('Ctrl Pts',(13.0508216223155,31.9791666734946,-48.706329375));
#14313=CARTESIAN_POINT('Ctrl Pts',(24.3531646875,31.7708333401613,-42.1809185638422));
#14314=CARTESIAN_POINT('Ctrl Pts',(35.6555077526845,31.562500006828,-35.6555077526845));
#14315=CARTESIAN_POINT('Ctrl Pts',(42.1809185638422,31.3541666734946,-24.3531646875));
#14316=CARTESIAN_POINT('Ctrl Pts',(48.706329375,31.1458333401613,-13.0508216223155));
#14317=CARTESIAN_POINT('Ctrl Pts',(48.706329375,30.937500006828,1.293339198242E-14));
#14318=CARTESIAN_POINT('Ctrl Pts',(48.706329375,30.7291666734946,13.0508216223155));
#14319=CARTESIAN_POINT('Ctrl Pts',(42.1809185638422,30.5208333401613,24.3531646875));
#14320=CARTESIAN_POINT('Ctrl Pts',(35.6555077526845,30.312500006828,35.6555077526845));
#14321=CARTESIAN_POINT('Ctrl Pts',(24.3531646875,30.1041666734946,42.1809185638422));
#14322=CARTESIAN_POINT('Ctrl Pts',(13.0508216223155,29.8958333401613,48.706329375));
#14323=CARTESIAN_POINT('Ctrl Pts',(-9.95098946405443E-15,29.687500006828,
48.706329375));
#14324=CARTESIAN_POINT('Ctrl Pts',(-13.0508216223155,29.4791666734946,48.706329375));
#14325=CARTESIAN_POINT('Ctrl Pts',(-24.3531646875,29.2708333401613,42.1809185638423));
#14326=CARTESIAN_POINT('Ctrl Pts',(-35.6555077526845,29.062500006828,35.6555077526845));
#14327=CARTESIAN_POINT('Ctrl Pts',(-42.1809185638422,28.8541666734946,24.3531646875));
#14328=CARTESIAN_POINT('Ctrl Pts',(-48.706329375,28.6458333401613,13.0508216223155));
#14329=CARTESIAN_POINT('Ctrl Pts',(-48.706329375,28.437500006828,-1.8898197019151E-14));
#14330=CARTESIAN_POINT('Ctrl Pts',(-46.,60.,0.));
#14331=CARTESIAN_POINT('Ctrl Pts',(-46.,59.7916666666667,-12.3256628518316));
#14332=CARTESIAN_POINT('Ctrl Pts',(-39.8371685740842,59.5833333333333,-23.));
#14333=CARTESIAN_POINT('Ctrl Pts',(-33.6743371481684,59.375,-33.6743371481684));
#14334=CARTESIAN_POINT('Ctrl Pts',(-23.,59.1666666666667,-39.8371685740842));
#14335=CARTESIAN_POINT('Ctrl Pts',(-12.3256628518317,58.9583333333333,-46.));
#14336=CARTESIAN_POINT('Ctrl Pts',(-2.81668763803891E-15,58.75,-46.));
#14337=CARTESIAN_POINT('Ctrl Pts',(12.3256628518316,58.5416666666667,-46.));
#14338=CARTESIAN_POINT('Ctrl Pts',(23.,58.3333333333333,-39.8371685740842));
#14339=CARTESIAN_POINT('Ctrl Pts',(33.6743371481683,58.125,-33.6743371481684));
#14340=CARTESIAN_POINT('Ctrl Pts',(39.8371685740842,57.9166666666667,-23.));
#14341=CARTESIAN_POINT('Ctrl Pts',(46.,57.7083333333333,-12.3256628518317));
#14342=CARTESIAN_POINT('Ctrl Pts',(46.,57.5,-5.63337527607782E-15));
#14343=CARTESIAN_POINT('Ctrl Pts',(46.,57.2916666666667,12.3256628518316));
#14344=CARTESIAN_POINT('Ctrl Pts',(39.8371685740842,57.0833333333333,23.));
#14345=CARTESIAN_POINT('Ctrl Pts',(33.6743371481684,56.875,33.6743371481683));
#14346=CARTESIAN_POINT('Ctrl Pts',(23.,56.6666666666667,39.8371685740842));
#14347=CARTESIAN_POINT('Ctrl Pts',(12.3256628518317,56.4583333333333,46.));
#14348=CARTESIAN_POINT('Ctrl Pts',(8.45006291411674E-15,56.25,46.));
#14349=CARTESIAN_POINT('Ctrl Pts',(-12.3256628518316,56.0416666666667,46.));
#14350=CARTESIAN_POINT('Ctrl Pts',(-23.,55.8333333333333,39.8371685740842));
#14351=CARTESIAN_POINT('Ctrl Pts',(-33.6743371481683,55.625,33.6743371481684));
#14352=CARTESIAN_POINT('Ctrl Pts',(-39.8371685740842,55.4166666666667,23.));
#14353=CARTESIAN_POINT('Ctrl Pts',(-46.,55.2083333333333,12.3256628518317));
#14354=CARTESIAN_POINT('Ctrl Pts',(-46.,55.,0.));
#14355=CARTESIAN_POINT('Ctrl Pts',(-46.,54.7916666666667,-12.3256628518316));
#14356=CARTESIAN_POINT('Ctrl Pts',(-39.8371685740842,54.5833333333333,-23.));
#14357=CARTESIAN_POINT('Ctrl Pts',(-33.6743371481684,54.375,-33.6743371481684));
#14358=CARTESIAN_POINT('Ctrl Pts',(-23.,54.1666666666667,-39.8371685740842));
#14359=CARTESIAN_POINT('Ctrl Pts',(-12.3256628518317,53.9583333333333,-46.));
#14360=CARTESIAN_POINT('Ctrl Pts',(-2.81668763803891E-15,53.75,-46.));
#14361=CARTESIAN_POINT('Ctrl Pts',(12.3256628518316,53.5416666666667,-46.));
#14362=CARTESIAN_POINT('Ctrl Pts',(23.,53.3333333333333,-39.8371685740842));
#14363=CARTESIAN_POINT('Ctrl Pts',(33.6743371481683,53.125,-33.6743371481684));
#14364=CARTESIAN_POINT('Ctrl Pts',(39.8371685740842,52.9166666666667,-23.));
#14365=CARTESIAN_POINT('Ctrl Pts',(46.,52.7083333333333,-12.3256628518317));
#14366=CARTESIAN_POINT('Ctrl Pts',(46.,52.5,-5.63337527607782E-15));
#14367=CARTESIAN_POINT('Ctrl Pts',(46.,52.2916666666667,12.3256628518316));
#14368=CARTESIAN_POINT('Ctrl Pts',(39.8371685740842,52.0833333333333,23.));
#14369=CARTESIAN_POINT('Ctrl Pts',(33.6743371481684,51.875,33.6743371481683));
#14370=CARTESIAN_POINT('Ctrl Pts',(23.,51.6666666666667,39.8371685740842));
#14371=CARTESIAN_POINT('Ctrl Pts',(12.3256628518317,51.4583333333333,46.));
#14372=CARTESIAN_POINT('Ctrl Pts',(8.45006291411674E-15,51.25,46.));
#14373=CARTESIAN_POINT('Ctrl Pts',(-12.3256628518316,51.0416666666667,46.));
#14374=CARTESIAN_POINT('Ctrl Pts',(-23.,50.8333333333333,39.8371685740842));
#14375=CARTESIAN_POINT('Ctrl Pts',(-33.6743371481683,50.625,33.6743371481684));
#14376=CARTESIAN_POINT('Ctrl Pts',(-39.8371685740842,50.4166666666667,23.));
#14377=CARTESIAN_POINT('Ctrl Pts',(-46.,50.2083333333333,12.3256628518317));
#14378=CARTESIAN_POINT('Ctrl Pts',(-46.,50.,0.));
#14379=CARTESIAN_POINT('Ctrl Pts',(-46.,49.7916666666667,-12.3256628518316));
#14380=CARTESIAN_POINT('Ctrl Pts',(-39.8371685740842,49.5833333333333,-23.));
#14381=CARTESIAN_POINT('Ctrl Pts',(-33.6743371481684,49.375,-33.6743371481684));
#14382=CARTESIAN_POINT('Ctrl Pts',(-23.,49.1666666666667,-39.8371685740842));
#14383=CARTESIAN_POINT('Ctrl Pts',(-12.3256628518317,48.9583333333333,-46.));
#14384=CARTESIAN_POINT('Ctrl Pts',(-2.81668763803891E-15,48.75,-46.));
#14385=CARTESIAN_POINT('Ctrl Pts',(12.3256628518316,48.5416666666667,-46.));
#14386=CARTESIAN_POINT('Ctrl Pts',(23.,48.3333333333333,-39.8371685740842));
#14387=CARTESIAN_POINT('Ctrl Pts',(33.6743371481683,48.125,-33.6743371481684));
#14388=CARTESIAN_POINT('Ctrl Pts',(39.8371685740842,47.9166666666667,-23.));
#14389=CARTESIAN_POINT('Ctrl Pts',(46.,47.7083333333333,-12.3256628518317));
#14390=CARTESIAN_POINT('Ctrl Pts',(46.,47.5,-5.63337527607782E-15));
#14391=CARTESIAN_POINT('Ctrl Pts',(46.,47.2916666666667,12.3256628518316));
#14392=CARTESIAN_POINT('Ctrl Pts',(39.8371685740842,47.0833333333333,23.));
#14393=CARTESIAN_POINT('Ctrl Pts',(33.6743371481684,46.875,33.6743371481683));
#14394=CARTESIAN_POINT('Ctrl Pts',(23.,46.6666666666667,39.8371685740842));
#14395=CARTESIAN_POINT('Ctrl Pts',(12.3256628518317,46.4583333333333,46.));
#14396=CARTESIAN_POINT('Ctrl Pts',(8.45006291411674E-15,46.25,46.));
#14397=CARTESIAN_POINT('Ctrl Pts',(-12.3256628518316,46.0416666666667,46.));
#14398=CARTESIAN_POINT('Ctrl Pts',(-23.,45.8333333333333,39.8371685740842));
#14399=CARTESIAN_POINT('Ctrl Pts',(-33.6743371481683,45.625,33.6743371481684));
#14400=CARTESIAN_POINT('Ctrl Pts',(-39.8371685740842,45.4166666666667,23.));
#14401=CARTESIAN_POINT('Ctrl Pts',(-46.,45.2083333333333,12.3256628518317));
#14402=CARTESIAN_POINT('Ctrl Pts',(-46.,45.,0.));
#14403=CARTESIAN_POINT('Ctrl Pts',(-46.,44.7916666666667,-12.3256628518316));
#14404=CARTESIAN_POINT('Ctrl Pts',(-39.8371685740842,44.5833333333333,-23.));
#14405=CARTESIAN_POINT('Ctrl Pts',(-33.6743371481684,44.375,-33.6743371481684));
#14406=CARTESIAN_POINT('Ctrl Pts',(-23.,44.1666666666667,-39.8371685740842));
#14407=CARTESIAN_POINT('Ctrl Pts',(-12.3256628518317,43.9583333333333,-46.));
#14408=CARTESIAN_POINT('Ctrl Pts',(-2.81668763803891E-15,43.75,-46.));
#14409=CARTESIAN_POINT('Ctrl Pts',(12.3256628518316,43.5416666666667,-46.));
#14410=CARTESIAN_POINT('Ctrl Pts',(23.,43.3333333333333,-39.8371685740842));
#14411=CARTESIAN_POINT('Ctrl Pts',(33.6743371481683,43.125,-33.6743371481684));
#14412=CARTESIAN_POINT('Ctrl Pts',(39.8371685740842,42.9166666666667,-23.));
#14413=CARTESIAN_POINT('Ctrl Pts',(46.,42.7083333333333,-12.3256628518317));
#14414=CARTESIAN_POINT('Ctrl Pts',(46.,42.5,-5.63337527607782E-15));
#14415=CARTESIAN_POINT('Ctrl Pts',(46.,42.2916666666667,12.3256628518316));
#14416=CARTESIAN_POINT('Ctrl Pts',(39.8371685740842,42.0833333333333,23.));
#14417=CARTESIAN_POINT('Ctrl Pts',(33.6743371481684,41.875,33.6743371481683));
#14418=CARTESIAN_POINT('Ctrl Pts',(23.,41.6666666666667,39.8371685740842));
#14419=CARTESIAN_POINT('Ctrl Pts',(12.3256628518317,41.4583333333333,46.));
#14420=CARTESIAN_POINT('Ctrl Pts',(8.45006291411674E-15,41.25,46.));
#14421=CARTESIAN_POINT('Ctrl Pts',(-12.3256628518316,41.0416666666667,46.));
#14422=CARTESIAN_POINT('Ctrl Pts',(-23.,40.8333333333333,39.8371685740842));
#14423=CARTESIAN_POINT('Ctrl Pts',(-33.6743371481683,40.625,33.6743371481684));
#14424=CARTESIAN_POINT('Ctrl Pts',(-39.8371685740842,40.4166666666667,23.));
#14425=CARTESIAN_POINT('Ctrl Pts',(-46.,40.2083333333333,12.3256628518317));
#14426=CARTESIAN_POINT('Ctrl Pts',(-46.,40.,0.));
#14427=CARTESIAN_POINT('Ctrl Pts',(-46.,39.7916666666667,-12.3256628518316));
#14428=CARTESIAN_POINT('Ctrl Pts',(-39.8371685740842,39.5833333333333,-23.));
#14429=CARTESIAN_POINT('Ctrl Pts',(-33.6743371481684,39.375,-33.6743371481684));
#14430=CARTESIAN_POINT('Ctrl Pts',(-23.,39.1666666666667,-39.8371685740842));
#14431=CARTESIAN_POINT('Ctrl Pts',(-12.3256628518317,38.9583333333333,-46.));
#14432=CARTESIAN_POINT('Ctrl Pts',(-2.81668763803891E-15,38.75,-46.));
#14433=CARTESIAN_POINT('Ctrl Pts',(12.3256628518316,38.5416666666667,-46.));
#14434=CARTESIAN_POINT('Ctrl Pts',(23.,38.3333333333333,-39.8371685740842));
#14435=CARTESIAN_POINT('Ctrl Pts',(33.6743371481683,38.125,-33.6743371481684));
#14436=CARTESIAN_POINT('Ctrl Pts',(39.8371685740842,37.9166666666667,-23.));
#14437=CARTESIAN_POINT('Ctrl Pts',(46.,37.7083333333333,-12.3256628518317));
#14438=CARTESIAN_POINT('Ctrl Pts',(46.,37.5,-5.63337527607782E-15));
#14439=CARTESIAN_POINT('Ctrl Pts',(46.,37.2916666666667,12.3256628518316));
#14440=CARTESIAN_POINT('Ctrl Pts',(39.8371685740842,37.0833333333333,23.));
#14441=CARTESIAN_POINT('Ctrl Pts',(33.6743371481684,36.875,33.6743371481683));
#14442=CARTESIAN_POINT('Ctrl Pts',(23.,36.6666666666667,39.8371685740842));
#14443=CARTESIAN_POINT('Ctrl Pts',(12.3256628518317,36.4583333333333,46.));
#14444=CARTESIAN_POINT('Ctrl Pts',(8.45006291411674E-15,36.25,46.));
#14445=CARTESIAN_POINT('Ctrl Pts',(-12.3256628518316,36.0416666666667,46.));
#14446=CARTESIAN_POINT('Ctrl Pts',(-23.,35.8333333333333,39.8371685740842));
#14447=CARTESIAN_POINT('Ctrl Pts',(-33.6743371481683,35.625,33.6743371481684));
#14448=CARTESIAN_POINT('Ctrl Pts',(-39.8371685740842,35.4166666666667,23.));
#14449=CARTESIAN_POINT('Ctrl Pts',(-46.,35.2083333333333,12.3256628518317));
#14450=CARTESIAN_POINT('Ctrl Pts',(-46.,35.,0.));
#14451=CARTESIAN_POINT('Ctrl Pts',(-46.,34.7916666666667,-12.3256628518316));
#14452=CARTESIAN_POINT('Ctrl Pts',(-39.8371685740842,34.5833333333333,-23.));
#14453=CARTESIAN_POINT('Ctrl Pts',(-33.6743371481684,34.375,-33.6743371481684));
#14454=CARTESIAN_POINT('Ctrl Pts',(-23.,34.1666666666667,-39.8371685740842));
#14455=CARTESIAN_POINT('Ctrl Pts',(-12.3256628518317,33.9583333333333,-46.));
#14456=CARTESIAN_POINT('Ctrl Pts',(-2.81668763803891E-15,33.75,-46.));
#14457=CARTESIAN_POINT('Ctrl Pts',(12.3256628518316,33.5416666666667,-46.));
#14458=CARTESIAN_POINT('Ctrl Pts',(23.,33.3333333333333,-39.8371685740842));
#14459=CARTESIAN_POINT('Ctrl Pts',(33.6743371481683,33.125,-33.6743371481684));
#14460=CARTESIAN_POINT('Ctrl Pts',(39.8371685740842,32.9166666666667,-23.));
#14461=CARTESIAN_POINT('Ctrl Pts',(46.,32.7083333333333,-12.3256628518317));
#14462=CARTESIAN_POINT('Ctrl Pts',(46.,32.5,-5.63337527607782E-15));
#14463=CARTESIAN_POINT('Ctrl Pts',(46.,32.2916666666667,12.3256628518316));
#14464=CARTESIAN_POINT('Ctrl Pts',(39.8371685740842,32.0833333333333,23.));
#14465=CARTESIAN_POINT('Ctrl Pts',(33.6743371481684,31.875,33.6743371481683));
#14466=CARTESIAN_POINT('Ctrl Pts',(23.,31.6666666666667,39.8371685740842));
#14467=CARTESIAN_POINT('Ctrl Pts',(12.3256628518317,31.4583333333333,46.));
#14468=CARTESIAN_POINT('Ctrl Pts',(8.45006291411674E-15,31.25,46.));
#14469=CARTESIAN_POINT('Ctrl Pts',(-12.3256628518316,31.0416666666667,46.));
#14470=CARTESIAN_POINT('Ctrl Pts',(-23.,30.8333333333333,39.8371685740842));
#14471=CARTESIAN_POINT('Ctrl Pts',(-33.6743371481683,30.625,33.6743371481684));
#14472=CARTESIAN_POINT('Ctrl Pts',(-39.8371685740842,30.4166666666667,23.));
#14473=CARTESIAN_POINT('Ctrl Pts',(-46.,30.2083333333333,12.3256628518317));
#14474=CARTESIAN_POINT('Ctrl Pts',(-46.,30.,0.));
#14475=CARTESIAN_POINT('Ctrl Pts',(-45.858362923034,55.061608680256,3.60701400320327));
#14476=CARTESIAN_POINT('Ctrl Pts',(-46.089925771934,54.9280150456297,3.60701400320327));
#14477=CARTESIAN_POINT('Ctrl Pts',(-46.5530501979845,54.6608255719956,3.60701400320327));
#14478=CARTESIAN_POINT('Ctrl Pts',(-47.0161721905706,54.3936318804497,3.60701400320325));
#14479=CARTESIAN_POINT('Ctrl Pts',(-47.6893519862319,54.0052434879083,3.60701400320325));
#14480=CARTESIAN_POINT('Ctrl Pts',(-48.1309692507094,53.7504492807381,3.60701400320327));
#14481=CARTESIAN_POINT('Ctrl Pts',(-48.5725845633798,53.4956516907298,3.60701400320327));
#14482=CARTESIAN_POINT('Origin',(-4.32455831995572,-7916.57953929723,-4524.0108731871));
#14483=CARTESIAN_POINT('Ctrl Pts',(-48.706329375,58.437500006828,-1.8898197019151E-14));
#14484=CARTESIAN_POINT('Ctrl Pts',(-48.706329375,58.2291666734946,-13.0508216223155));
#14485=CARTESIAN_POINT('Ctrl Pts',(-42.1809185638422,58.0208333401613,-24.3531646875));
#14486=CARTESIAN_POINT('Ctrl Pts',(-35.6555077526845,57.812500006828,-35.6555077526845));
#14487=CARTESIAN_POINT('Ctrl Pts',(-24.3531646875,57.6041666734946,-42.1809185638422));
#14488=CARTESIAN_POINT('Ctrl Pts',(-13.0508216223155,57.3958333401613,-48.706329375));
#14489=CARTESIAN_POINT('Ctrl Pts',(1.59157945007855E-14,57.187500006828,
-48.706329375));
#14490=CARTESIAN_POINT('Ctrl Pts',(13.0508216223155,56.9791666734946,-48.706329375));
#14491=CARTESIAN_POINT('Ctrl Pts',(24.3531646875,56.7708333401613,-42.1809185638422));
#14492=CARTESIAN_POINT('Ctrl Pts',(35.6555077526845,56.562500006828,-35.6555077526845));
#14493=CARTESIAN_POINT('Ctrl Pts',(42.1809185638422,56.3541666734946,-24.3531646875));
#14494=CARTESIAN_POINT('Ctrl Pts',(48.706329375,56.1458333401613,-13.0508216223155));
#14495=CARTESIAN_POINT('Ctrl Pts',(48.706329375,55.937500006828,1.293339198242E-14));
#14496=CARTESIAN_POINT('Ctrl Pts',(48.706329375,55.7291666734946,13.0508216223155));
#14497=CARTESIAN_POINT('Ctrl Pts',(42.1809185638422,55.5208333401613,24.3531646875));
#14498=CARTESIAN_POINT('Ctrl Pts',(35.6555077526845,55.312500006828,35.6555077526845));
#14499=CARTESIAN_POINT('Ctrl Pts',(24.3531646875,55.1041666734946,42.1809185638422));
#14500=CARTESIAN_POINT('Ctrl Pts',(13.0508216223155,54.8958333401613,48.706329375));
#14501=CARTESIAN_POINT('Ctrl Pts',(-9.95098946405443E-15,54.687500006828,
48.706329375));
#14502=CARTESIAN_POINT('Ctrl Pts',(-13.0508216223155,54.4791666734946,48.706329375));
#14503=CARTESIAN_POINT('Ctrl Pts',(-24.3531646875,54.2708333401613,42.1809185638423));
#14504=CARTESIAN_POINT('Ctrl Pts',(-35.6555077526845,54.062500006828,35.6555077526845));
#14505=CARTESIAN_POINT('Ctrl Pts',(-42.1809185638422,53.8541666734946,24.3531646875));
#14506=CARTESIAN_POINT('Ctrl Pts',(-48.706329375,53.6458333401613,13.0508216223155));
#14507=CARTESIAN_POINT('Ctrl Pts',(-48.706329375,53.437500006828,-1.8898197019151E-14));
#14508=CARTESIAN_POINT('Ctrl Pts',(-48.706329375,53.2291666734946,-13.0508216223155));
#14509=CARTESIAN_POINT('Ctrl Pts',(-42.1809185638422,53.0208333401613,-24.3531646875));
#14510=CARTESIAN_POINT('Ctrl Pts',(-35.6555077526845,52.812500006828,-35.6555077526845));
#14511=CARTESIAN_POINT('Ctrl Pts',(-24.3531646875,52.6041666734946,-42.1809185638422));
#14512=CARTESIAN_POINT('Ctrl Pts',(-13.0508216223155,52.3958333401613,-48.706329375));
#14513=CARTESIAN_POINT('Ctrl Pts',(1.59157945007855E-14,52.187500006828,
-48.706329375));
#14514=CARTESIAN_POINT('Ctrl Pts',(13.0508216223155,51.9791666734946,-48.706329375));
#14515=CARTESIAN_POINT('Ctrl Pts',(24.3531646875,51.7708333401613,-42.1809185638422));
#14516=CARTESIAN_POINT('Ctrl Pts',(35.6555077526845,51.562500006828,-35.6555077526845));
#14517=CARTESIAN_POINT('Ctrl Pts',(42.1809185638422,51.3541666734946,-24.3531646875));
#14518=CARTESIAN_POINT('Ctrl Pts',(48.706329375,51.1458333401613,-13.0508216223155));
#14519=CARTESIAN_POINT('Ctrl Pts',(48.706329375,50.937500006828,1.293339198242E-14));
#14520=CARTESIAN_POINT('Ctrl Pts',(48.706329375,50.7291666734946,13.0508216223155));
#14521=CARTESIAN_POINT('Ctrl Pts',(42.1809185638422,50.5208333401613,24.3531646875));
#14522=CARTESIAN_POINT('Ctrl Pts',(35.6555077526845,50.312500006828,35.6555077526845));
#14523=CARTESIAN_POINT('Ctrl Pts',(24.3531646875,50.1041666734946,42.1809185638422));
#14524=CARTESIAN_POINT('Ctrl Pts',(13.0508216223155,49.8958333401613,48.706329375));
#14525=CARTESIAN_POINT('Ctrl Pts',(-9.95098946405443E-15,49.687500006828,
48.706329375));
#14526=CARTESIAN_POINT('Ctrl Pts',(-13.0508216223155,49.4791666734946,48.706329375));
#14527=CARTESIAN_POINT('Ctrl Pts',(-24.3531646875,49.2708333401613,42.1809185638423));
#14528=CARTESIAN_POINT('Ctrl Pts',(-35.6555077526845,49.062500006828,35.6555077526845));
#14529=CARTESIAN_POINT('Ctrl Pts',(-42.1809185638422,48.8541666734946,24.3531646875));
#14530=CARTESIAN_POINT('Ctrl Pts',(-48.706329375,48.6458333401613,13.0508216223155));
#14531=CARTESIAN_POINT('Ctrl Pts',(-48.706329375,48.437500006828,-1.8898197019151E-14));
#14532=CARTESIAN_POINT('Ctrl Pts',(-48.706329375,48.2291666734946,-13.0508216223155));
#14533=CARTESIAN_POINT('Ctrl Pts',(-42.1809185638422,48.0208333401613,-24.3531646875));
#14534=CARTESIAN_POINT('Ctrl Pts',(-35.6555077526845,47.812500006828,-35.6555077526845));
#14535=CARTESIAN_POINT('Ctrl Pts',(-24.3531646875,47.6041666734946,-42.1809185638422));
#14536=CARTESIAN_POINT('Ctrl Pts',(-13.0508216223155,47.3958333401613,-48.706329375));
#14537=CARTESIAN_POINT('Ctrl Pts',(1.59157945007855E-14,47.187500006828,
-48.706329375));
#14538=CARTESIAN_POINT('Ctrl Pts',(13.0508216223155,46.9791666734946,-48.706329375));
#14539=CARTESIAN_POINT('Ctrl Pts',(24.3531646875,46.7708333401613,-42.1809185638422));
#14540=CARTESIAN_POINT('Ctrl Pts',(35.6555077526845,46.562500006828,-35.6555077526845));
#14541=CARTESIAN_POINT('Ctrl Pts',(42.1809185638422,46.3541666734946,-24.3531646875));
#14542=CARTESIAN_POINT('Ctrl Pts',(48.706329375,46.1458333401613,-13.0508216223155));
#14543=CARTESIAN_POINT('Ctrl Pts',(48.706329375,45.937500006828,1.293339198242E-14));
#14544=CARTESIAN_POINT('Ctrl Pts',(48.706329375,45.7291666734946,13.0508216223155));
#14545=CARTESIAN_POINT('Ctrl Pts',(42.1809185638422,45.5208333401613,24.3531646875));
#14546=CARTESIAN_POINT('Ctrl Pts',(35.6555077526845,45.312500006828,35.6555077526845));
#14547=CARTESIAN_POINT('Ctrl Pts',(24.3531646875,45.1041666734946,42.1809185638422));
#14548=CARTESIAN_POINT('Ctrl Pts',(13.0508216223155,44.8958333401613,48.706329375));
#14549=CARTESIAN_POINT('Ctrl Pts',(-9.95098946405443E-15,44.687500006828,
48.706329375));
#14550=CARTESIAN_POINT('Ctrl Pts',(-13.0508216223155,44.4791666734946,48.706329375));
#14551=CARTESIAN_POINT('Ctrl Pts',(-24.3531646875,44.2708333401613,42.1809185638423));
#14552=CARTESIAN_POINT('Ctrl Pts',(-35.6555077526845,44.062500006828,35.6555077526845));
#14553=CARTESIAN_POINT('Ctrl Pts',(-42.1809185638422,43.8541666734946,24.3531646875));
#14554=CARTESIAN_POINT('Ctrl Pts',(-48.706329375,43.6458333401613,13.0508216223155));
#14555=CARTESIAN_POINT('Ctrl Pts',(-48.706329375,43.437500006828,-1.8898197019151E-14));
#14556=CARTESIAN_POINT('Ctrl Pts',(-48.706329375,43.2291666734946,-13.0508216223155));
#14557=CARTESIAN_POINT('Ctrl Pts',(-42.1809185638422,43.0208333401613,-24.3531646875));
#14558=CARTESIAN_POINT('Ctrl Pts',(-35.6555077526845,42.812500006828,-35.6555077526845));
#14559=CARTESIAN_POINT('Ctrl Pts',(-24.3531646875,42.6041666734946,-42.1809185638422));
#14560=CARTESIAN_POINT('Ctrl Pts',(-13.0508216223155,42.3958333401613,-48.706329375));
#14561=CARTESIAN_POINT('Ctrl Pts',(1.59157945007855E-14,42.187500006828,
-48.706329375));
#14562=CARTESIAN_POINT('Ctrl Pts',(13.0508216223155,41.9791666734946,-48.706329375));
#14563=CARTESIAN_POINT('Ctrl Pts',(24.3531646875,41.7708333401613,-42.1809185638422));
#14564=CARTESIAN_POINT('Ctrl Pts',(35.6555077526845,41.562500006828,-35.6555077526845));
#14565=CARTESIAN_POINT('Ctrl Pts',(42.1809185638422,41.3541666734946,-24.3531646875));
#14566=CARTESIAN_POINT('Ctrl Pts',(48.706329375,41.1458333401613,-13.0508216223155));
#14567=CARTESIAN_POINT('Ctrl Pts',(48.706329375,40.937500006828,1.293339198242E-14));
#14568=CARTESIAN_POINT('Ctrl Pts',(48.706329375,40.7291666734946,13.0508216223155));
#14569=CARTESIAN_POINT('Ctrl Pts',(42.1809185638422,40.5208333401613,24.3531646875));
#14570=CARTESIAN_POINT('Ctrl Pts',(35.6555077526845,40.312500006828,35.6555077526845));
#14571=CARTESIAN_POINT('Ctrl Pts',(24.3531646875,40.1041666734946,42.1809185638422));
#14572=CARTESIAN_POINT('Ctrl Pts',(13.0508216223155,39.8958333401613,48.706329375));
#14573=CARTESIAN_POINT('Ctrl Pts',(-9.95098946405443E-15,39.687500006828,
48.706329375));
#14574=CARTESIAN_POINT('Ctrl Pts',(-13.0508216223155,39.4791666734946,48.706329375));
#14575=CARTESIAN_POINT('Ctrl Pts',(-24.3531646875,39.2708333401613,42.1809185638423));
#14576=CARTESIAN_POINT('Ctrl Pts',(-35.6555077526845,39.062500006828,35.6555077526845));
#14577=CARTESIAN_POINT('Ctrl Pts',(-42.1809185638422,38.8541666734946,24.3531646875));
#14578=CARTESIAN_POINT('Ctrl Pts',(-48.706329375,38.6458333401613,13.0508216223155));
#14579=CARTESIAN_POINT('Ctrl Pts',(-48.706329375,38.437500006828,-1.8898197019151E-14));
#14580=CARTESIAN_POINT('Ctrl Pts',(-48.706329375,38.2291666734946,-13.0508216223155));
#14581=CARTESIAN_POINT('Ctrl Pts',(-42.1809185638422,38.0208333401613,-24.3531646875));
#14582=CARTESIAN_POINT('Ctrl Pts',(-35.6555077526845,37.812500006828,-35.6555077526845));
#14583=CARTESIAN_POINT('Ctrl Pts',(-24.3531646875,37.6041666734946,-42.1809185638422));
#14584=CARTESIAN_POINT('Ctrl Pts',(-13.0508216223155,37.3958333401613,-48.706329375));
#14585=CARTESIAN_POINT('Ctrl Pts',(1.59157945007855E-14,37.187500006828,
-48.706329375));
#14586=CARTESIAN_POINT('Ctrl Pts',(13.0508216223155,36.9791666734946,-48.706329375));
#14587=CARTESIAN_POINT('Ctrl Pts',(24.3531646875,36.7708333401613,-42.1809185638422));
#14588=CARTESIAN_POINT('Ctrl Pts',(35.6555077526845,36.562500006828,-35.6555077526845));
#14589=CARTESIAN_POINT('Ctrl Pts',(42.1809185638422,36.3541666734946,-24.3531646875));
#14590=CARTESIAN_POINT('Ctrl Pts',(48.706329375,36.1458333401613,-13.0508216223155));
#14591=CARTESIAN_POINT('Ctrl Pts',(48.706329375,35.937500006828,1.293339198242E-14));
#14592=CARTESIAN_POINT('Ctrl Pts',(48.706329375,35.7291666734946,13.0508216223155));
#14593=CARTESIAN_POINT('Ctrl Pts',(42.1809185638422,35.5208333401613,24.3531646875));
#14594=CARTESIAN_POINT('Ctrl Pts',(35.6555077526845,35.312500006828,35.6555077526845));
#14595=CARTESIAN_POINT('Ctrl Pts',(24.3531646875,35.1041666734946,42.1809185638422));
#14596=CARTESIAN_POINT('Ctrl Pts',(13.0508216223155,34.8958333401613,48.706329375));
#14597=CARTESIAN_POINT('Ctrl Pts',(-9.95098946405443E-15,34.687500006828,
48.706329375));
#14598=CARTESIAN_POINT('Ctrl Pts',(-13.0508216223155,34.4791666734946,48.706329375));
#14599=CARTESIAN_POINT('Ctrl Pts',(-24.3531646875,34.2708333401613,42.1809185638423));
#14600=CARTESIAN_POINT('Ctrl Pts',(-35.6555077526845,34.062500006828,35.6555077526845));
#14601=CARTESIAN_POINT('Ctrl Pts',(-42.1809185638422,33.8541666734946,24.3531646875));
#14602=CARTESIAN_POINT('Ctrl Pts',(-48.706329375,33.6458333401613,13.0508216223155));
#14603=CARTESIAN_POINT('Ctrl Pts',(-48.706329375,33.437500006828,-1.8898197019151E-14));
#14604=CARTESIAN_POINT('Ctrl Pts',(-48.706329375,33.2291666734946,-13.0508216223155));
#14605=CARTESIAN_POINT('Ctrl Pts',(-42.1809185638422,33.0208333401613,-24.3531646875));
#14606=CARTESIAN_POINT('Ctrl Pts',(-35.6555077526845,32.812500006828,-35.6555077526845));
#14607=CARTESIAN_POINT('Ctrl Pts',(-24.3531646875,32.6041666734946,-42.1809185638422));
#14608=CARTESIAN_POINT('Ctrl Pts',(-13.0508216223155,32.3958333401613,-48.706329375));
#14609=CARTESIAN_POINT('Ctrl Pts',(1.59157945007855E-14,32.187500006828,
-48.706329375));
#14610=CARTESIAN_POINT('Ctrl Pts',(13.0508216223155,31.9791666734946,-48.706329375));
#14611=CARTESIAN_POINT('Ctrl Pts',(24.3531646875,31.7708333401613,-42.1809185638422));
#14612=CARTESIAN_POINT('Ctrl Pts',(35.6555077526845,31.562500006828,-35.6555077526845));
#14613=CARTESIAN_POINT('Ctrl Pts',(42.1809185638422,31.3541666734946,-24.3531646875));
#14614=CARTESIAN_POINT('Ctrl Pts',(48.706329375,31.1458333401613,-13.0508216223155));
#14615=CARTESIAN_POINT('Ctrl Pts',(48.706329375,30.937500006828,1.293339198242E-14));
#14616=CARTESIAN_POINT('Ctrl Pts',(48.706329375,30.7291666734946,13.0508216223155));
#14617=CARTESIAN_POINT('Ctrl Pts',(42.1809185638422,30.5208333401613,24.3531646875));
#14618=CARTESIAN_POINT('Ctrl Pts',(35.6555077526845,30.312500006828,35.6555077526845));
#14619=CARTESIAN_POINT('Ctrl Pts',(24.3531646875,30.1041666734946,42.1809185638422));
#14620=CARTESIAN_POINT('Ctrl Pts',(13.0508216223155,29.8958333401613,48.706329375));
#14621=CARTESIAN_POINT('Ctrl Pts',(-9.95098946405443E-15,29.687500006828,
48.706329375));
#14622=CARTESIAN_POINT('Ctrl Pts',(-13.0508216223155,29.4791666734946,48.706329375));
#14623=CARTESIAN_POINT('Ctrl Pts',(-24.3531646875,29.2708333401613,42.1809185638423));
#14624=CARTESIAN_POINT('Ctrl Pts',(-35.6555077526845,29.062500006828,35.6555077526845));
#14625=CARTESIAN_POINT('Ctrl Pts',(-42.1809185638422,28.8541666734946,24.3531646875));
#14626=CARTESIAN_POINT('Ctrl Pts',(-48.706329375,28.6458333401613,13.0508216223155));
#14627=CARTESIAN_POINT('Ctrl Pts',(-48.706329375,28.437500006828,-1.8898197019151E-14));
#14628=CARTESIAN_POINT('Ctrl Pts',(-46.,60.,0.));
#14629=CARTESIAN_POINT('Ctrl Pts',(-46.,59.7916666666667,-12.3256628518316));
#14630=CARTESIAN_POINT('Ctrl Pts',(-39.8371685740842,59.5833333333333,-23.));
#14631=CARTESIAN_POINT('Ctrl Pts',(-33.6743371481684,59.375,-33.6743371481684));
#14632=CARTESIAN_POINT('Ctrl Pts',(-23.,59.1666666666667,-39.8371685740842));
#14633=CARTESIAN_POINT('Ctrl Pts',(-12.3256628518317,58.9583333333333,-46.));
#14634=CARTESIAN_POINT('Ctrl Pts',(-2.81668763803891E-15,58.75,-46.));
#14635=CARTESIAN_POINT('Ctrl Pts',(12.3256628518316,58.5416666666667,-46.));
#14636=CARTESIAN_POINT('Ctrl Pts',(23.,58.3333333333333,-39.8371685740842));
#14637=CARTESIAN_POINT('Ctrl Pts',(33.6743371481683,58.125,-33.6743371481684));
#14638=CARTESIAN_POINT('Ctrl Pts',(39.8371685740842,57.9166666666667,-23.));
#14639=CARTESIAN_POINT('Ctrl Pts',(46.,57.7083333333333,-12.3256628518317));
#14640=CARTESIAN_POINT('Ctrl Pts',(46.,57.5,-5.63337527607782E-15));
#14641=CARTESIAN_POINT('Ctrl Pts',(46.,57.2916666666667,12.3256628518316));
#14642=CARTESIAN_POINT('Ctrl Pts',(39.8371685740842,57.0833333333333,23.));
#14643=CARTESIAN_POINT('Ctrl Pts',(33.6743371481684,56.875,33.6743371481683));
#14644=CARTESIAN_POINT('Ctrl Pts',(23.,56.6666666666667,39.8371685740842));
#14645=CARTESIAN_POINT('Ctrl Pts',(12.3256628518317,56.4583333333333,46.));
#14646=CARTESIAN_POINT('Ctrl Pts',(8.45006291411674E-15,56.25,46.));
#14647=CARTESIAN_POINT('Ctrl Pts',(-12.3256628518316,56.0416666666667,46.));
#14648=CARTESIAN_POINT('Ctrl Pts',(-23.,55.8333333333333,39.8371685740842));
#14649=CARTESIAN_POINT('Ctrl Pts',(-33.6743371481683,55.625,33.6743371481684));
#14650=CARTESIAN_POINT('Ctrl Pts',(-39.8371685740842,55.4166666666667,23.));
#14651=CARTESIAN_POINT('Ctrl Pts',(-46.,55.2083333333333,12.3256628518317));
#14652=CARTESIAN_POINT('Ctrl Pts',(-46.,55.,0.));
#14653=CARTESIAN_POINT('Ctrl Pts',(-46.,54.7916666666667,-12.3256628518316));
#14654=CARTESIAN_POINT('Ctrl Pts',(-39.8371685740842,54.5833333333333,-23.));
#14655=CARTESIAN_POINT('Ctrl Pts',(-33.6743371481684,54.375,-33.6743371481684));
#14656=CARTESIAN_POINT('Ctrl Pts',(-23.,54.1666666666667,-39.8371685740842));
#14657=CARTESIAN_POINT('Ctrl Pts',(-12.3256628518317,53.9583333333333,-46.));
#14658=CARTESIAN_POINT('Ctrl Pts',(-2.81668763803891E-15,53.75,-46.));
#14659=CARTESIAN_POINT('Ctrl Pts',(12.3256628518316,53.5416666666667,-46.));
#14660=CARTESIAN_POINT('Ctrl Pts',(23.,53.3333333333333,-39.8371685740842));
#14661=CARTESIAN_POINT('Ctrl Pts',(33.6743371481683,53.125,-33.6743371481684));
#14662=CARTESIAN_POINT('Ctrl Pts',(39.8371685740842,52.9166666666667,-23.));
#14663=CARTESIAN_POINT('Ctrl Pts',(46.,52.7083333333333,-12.3256628518317));
#14664=CARTESIAN_POINT('Ctrl Pts',(46.,52.5,-5.63337527607782E-15));
#14665=CARTESIAN_POINT('Ctrl Pts',(46.,52.2916666666667,12.3256628518316));
#14666=CARTESIAN_POINT('Ctrl Pts',(39.8371685740842,52.0833333333333,23.));
#14667=CARTESIAN_POINT('Ctrl Pts',(33.6743371481684,51.875,33.6743371481683));
#14668=CARTESIAN_POINT('Ctrl Pts',(23.,51.6666666666667,39.8371685740842));
#14669=CARTESIAN_POINT('Ctrl Pts',(12.3256628518317,51.4583333333333,46.));
#14670=CARTESIAN_POINT('Ctrl Pts',(8.45006291411674E-15,51.25,46.));
#14671=CARTESIAN_POINT('Ctrl Pts',(-12.3256628518316,51.0416666666667,46.));
#14672=CARTESIAN_POINT('Ctrl Pts',(-23.,50.8333333333333,39.8371685740842));
#14673=CARTESIAN_POINT('Ctrl Pts',(-33.6743371481683,50.625,33.6743371481684));
#14674=CARTESIAN_POINT('Ctrl Pts',(-39.8371685740842,50.4166666666667,23.));
#14675=CARTESIAN_POINT('Ctrl Pts',(-46.,50.2083333333333,12.3256628518317));
#14676=CARTESIAN_POINT('Ctrl Pts',(-46.,50.,0.));
#14677=CARTESIAN_POINT('Ctrl Pts',(-46.,49.7916666666667,-12.3256628518316));
#14678=CARTESIAN_POINT('Ctrl Pts',(-39.8371685740842,49.5833333333333,-23.));
#14679=CARTESIAN_POINT('Ctrl Pts',(-33.6743371481684,49.375,-33.6743371481684));
#14680=CARTESIAN_POINT('Ctrl Pts',(-23.,49.1666666666667,-39.8371685740842));
#14681=CARTESIAN_POINT('Ctrl Pts',(-12.3256628518317,48.9583333333333,-46.));
#14682=CARTESIAN_POINT('Ctrl Pts',(-2.81668763803891E-15,48.75,-46.));
#14683=CARTESIAN_POINT('Ctrl Pts',(12.3256628518316,48.5416666666667,-46.));
#14684=CARTESIAN_POINT('Ctrl Pts',(23.,48.3333333333333,-39.8371685740842));
#14685=CARTESIAN_POINT('Ctrl Pts',(33.6743371481683,48.125,-33.6743371481684));
#14686=CARTESIAN_POINT('Ctrl Pts',(39.8371685740842,47.9166666666667,-23.));
#14687=CARTESIAN_POINT('Ctrl Pts',(46.,47.7083333333333,-12.3256628518317));
#14688=CARTESIAN_POINT('Ctrl Pts',(46.,47.5,-5.63337527607782E-15));
#14689=CARTESIAN_POINT('Ctrl Pts',(46.,47.2916666666667,12.3256628518316));
#14690=CARTESIAN_POINT('Ctrl Pts',(39.8371685740842,47.0833333333333,23.));
#14691=CARTESIAN_POINT('Ctrl Pts',(33.6743371481684,46.875,33.6743371481683));
#14692=CARTESIAN_POINT('Ctrl Pts',(23.,46.6666666666667,39.8371685740842));
#14693=CARTESIAN_POINT('Ctrl Pts',(12.3256628518317,46.4583333333333,46.));
#14694=CARTESIAN_POINT('Ctrl Pts',(8.45006291411674E-15,46.25,46.));
#14695=CARTESIAN_POINT('Ctrl Pts',(-12.3256628518316,46.0416666666667,46.));
#14696=CARTESIAN_POINT('Ctrl Pts',(-23.,45.8333333333333,39.8371685740842));
#14697=CARTESIAN_POINT('Ctrl Pts',(-33.6743371481683,45.625,33.6743371481684));
#14698=CARTESIAN_POINT('Ctrl Pts',(-39.8371685740842,45.4166666666667,23.));
#14699=CARTESIAN_POINT('Ctrl Pts',(-46.,45.2083333333333,12.3256628518317));
#14700=CARTESIAN_POINT('Ctrl Pts',(-46.,45.,0.));
#14701=CARTESIAN_POINT('Ctrl Pts',(-46.,44.7916666666667,-12.3256628518316));
#14702=CARTESIAN_POINT('Ctrl Pts',(-39.8371685740842,44.5833333333333,-23.));
#14703=CARTESIAN_POINT('Ctrl Pts',(-33.6743371481684,44.375,-33.6743371481684));
#14704=CARTESIAN_POINT('Ctrl Pts',(-23.,44.1666666666667,-39.8371685740842));
#14705=CARTESIAN_POINT('Ctrl Pts',(-12.3256628518317,43.9583333333333,-46.));
#14706=CARTESIAN_POINT('Ctrl Pts',(-2.81668763803891E-15,43.75,-46.));
#14707=CARTESIAN_POINT('Ctrl Pts',(12.3256628518316,43.5416666666667,-46.));
#14708=CARTESIAN_POINT('Ctrl Pts',(23.,43.3333333333333,-39.8371685740842));
#14709=CARTESIAN_POINT('Ctrl Pts',(33.6743371481683,43.125,-33.6743371481684));
#14710=CARTESIAN_POINT('Ctrl Pts',(39.8371685740842,42.9166666666667,-23.));
#14711=CARTESIAN_POINT('Ctrl Pts',(46.,42.7083333333333,-12.3256628518317));
#14712=CARTESIAN_POINT('Ctrl Pts',(46.,42.5,-5.63337527607782E-15));
#14713=CARTESIAN_POINT('Ctrl Pts',(46.,42.2916666666667,12.3256628518316));
#14714=CARTESIAN_POINT('Ctrl Pts',(39.8371685740842,42.0833333333333,23.));
#14715=CARTESIAN_POINT('Ctrl Pts',(33.6743371481684,41.875,33.6743371481683));
#14716=CARTESIAN_POINT('Ctrl Pts',(23.,41.6666666666667,39.8371685740842));
#14717=CARTESIAN_POINT('Ctrl Pts',(12.3256628518317,41.4583333333333,46.));
#14718=CARTESIAN_POINT('Ctrl Pts',(8.45006291411674E-15,41.25,46.));
#14719=CARTESIAN_POINT('Ctrl Pts',(-12.3256628518316,41.0416666666667,46.));
#14720=CARTESIAN_POINT('Ctrl Pts',(-23.,40.8333333333333,39.8371685740842));
#14721=CARTESIAN_POINT('Ctrl Pts',(-33.6743371481683,40.625,33.6743371481684));
#14722=CARTESIAN_POINT('Ctrl Pts',(-39.8371685740842,40.4166666666667,23.));
#14723=CARTESIAN_POINT('Ctrl Pts',(-46.,40.2083333333333,12.3256628518317));
#14724=CARTESIAN_POINT('Ctrl Pts',(-46.,40.,0.));
#14725=CARTESIAN_POINT('Ctrl Pts',(-46.,39.7916666666667,-12.3256628518316));
#14726=CARTESIAN_POINT('Ctrl Pts',(-39.8371685740842,39.5833333333333,-23.));
#14727=CARTESIAN_POINT('Ctrl Pts',(-33.6743371481684,39.375,-33.6743371481684));
#14728=CARTESIAN_POINT('Ctrl Pts',(-23.,39.1666666666667,-39.8371685740842));
#14729=CARTESIAN_POINT('Ctrl Pts',(-12.3256628518317,38.9583333333333,-46.));
#14730=CARTESIAN_POINT('Ctrl Pts',(-2.81668763803891E-15,38.75,-46.));
#14731=CARTESIAN_POINT('Ctrl Pts',(12.3256628518316,38.5416666666667,-46.));
#14732=CARTESIAN_POINT('Ctrl Pts',(23.,38.3333333333333,-39.8371685740842));
#14733=CARTESIAN_POINT('Ctrl Pts',(33.6743371481683,38.125,-33.6743371481684));
#14734=CARTESIAN_POINT('Ctrl Pts',(39.8371685740842,37.9166666666667,-23.));
#14735=CARTESIAN_POINT('Ctrl Pts',(46.,37.7083333333333,-12.3256628518317));
#14736=CARTESIAN_POINT('Ctrl Pts',(46.,37.5,-5.63337527607782E-15));
#14737=CARTESIAN_POINT('Ctrl Pts',(46.,37.2916666666667,12.3256628518316));
#14738=CARTESIAN_POINT('Ctrl Pts',(39.8371685740842,37.0833333333333,23.));
#14739=CARTESIAN_POINT('Ctrl Pts',(33.6743371481684,36.875,33.6743371481683));
#14740=CARTESIAN_POINT('Ctrl Pts',(23.,36.6666666666667,39.8371685740842));
#14741=CARTESIAN_POINT('Ctrl Pts',(12.3256628518317,36.4583333333333,46.));
#14742=CARTESIAN_POINT('Ctrl Pts',(8.45006291411674E-15,36.25,46.));
#14743=CARTESIAN_POINT('Ctrl Pts',(-12.3256628518316,36.0416666666667,46.));
#14744=CARTESIAN_POINT('Ctrl Pts',(-23.,35.8333333333333,39.8371685740842));
#14745=CARTESIAN_POINT('Ctrl Pts',(-33.6743371481683,35.625,33.6743371481684));
#14746=CARTESIAN_POINT('Ctrl Pts',(-39.8371685740842,35.4166666666667,23.));
#14747=CARTESIAN_POINT('Ctrl Pts',(-46.,35.2083333333333,12.3256628518317));
#14748=CARTESIAN_POINT('Ctrl Pts',(-46.,35.,0.));
#14749=CARTESIAN_POINT('Ctrl Pts',(-46.,34.7916666666667,-12.3256628518316));
#14750=CARTESIAN_POINT('Ctrl Pts',(-39.8371685740842,34.5833333333333,-23.));
#14751=CARTESIAN_POINT('Ctrl Pts',(-33.6743371481684,34.375,-33.6743371481684));
#14752=CARTESIAN_POINT('Ctrl Pts',(-23.,34.1666666666667,-39.8371685740842));
#14753=CARTESIAN_POINT('Ctrl Pts',(-12.3256628518317,33.9583333333333,-46.));
#14754=CARTESIAN_POINT('Ctrl Pts',(-2.81668763803891E-15,33.75,-46.));
#14755=CARTESIAN_POINT('Ctrl Pts',(12.3256628518316,33.5416666666667,-46.));
#14756=CARTESIAN_POINT('Ctrl Pts',(23.,33.3333333333333,-39.8371685740842));
#14757=CARTESIAN_POINT('Ctrl Pts',(33.6743371481683,33.125,-33.6743371481684));
#14758=CARTESIAN_POINT('Ctrl Pts',(39.8371685740842,32.9166666666667,-23.));
#14759=CARTESIAN_POINT('Ctrl Pts',(46.,32.7083333333333,-12.3256628518317));
#14760=CARTESIAN_POINT('Ctrl Pts',(46.,32.5,-5.63337527607782E-15));
#14761=CARTESIAN_POINT('Ctrl Pts',(46.,32.2916666666667,12.3256628518316));
#14762=CARTESIAN_POINT('Ctrl Pts',(39.8371685740842,32.0833333333333,23.));
#14763=CARTESIAN_POINT('Ctrl Pts',(33.6743371481684,31.875,33.6743371481683));
#14764=CARTESIAN_POINT('Ctrl Pts',(23.,31.6666666666667,39.8371685740842));
#14765=CARTESIAN_POINT('Ctrl Pts',(12.3256628518317,31.4583333333333,46.));
#14766=CARTESIAN_POINT('Ctrl Pts',(8.45006291411674E-15,31.25,46.));
#14767=CARTESIAN_POINT('Ctrl Pts',(-12.3256628518316,31.0416666666667,46.));
#14768=CARTESIAN_POINT('Ctrl Pts',(-23.,30.8333333333333,39.8371685740842));
#14769=CARTESIAN_POINT('Ctrl Pts',(-33.6743371481683,30.625,33.6743371481684));
#14770=CARTESIAN_POINT('Ctrl Pts',(-39.8371685740842,30.4166666666667,23.));
#14771=CARTESIAN_POINT('Ctrl Pts',(-46.,30.2083333333333,12.3256628518317));
#14772=CARTESIAN_POINT('Ctrl Pts',(-46.,30.,0.));
#14773=CARTESIAN_POINT('Origin',(4513.80899862641,-7905.15855185603,-4.33048603483869));
#14774=CARTESIAN_POINT('Ctrl Pts',(-4.32456003949879,48.8240181593938,-45.7962681936506));
#14775=CARTESIAN_POINT('Ctrl Pts',(-4.32456003949874,48.6905125468623,-46.0278818021281));
#14776=CARTESIAN_POINT('Ctrl Pts',(-4.3245600394988,48.4234964717135,-46.4911062234486));
#14777=CARTESIAN_POINT('Ctrl Pts',(-4.32456003949883,48.1564711191154,-46.954325296818));
#14778=CARTESIAN_POINT('Ctrl Pts',(-4.32456003949883,47.7677643029224,-47.6286149142205));
#14779=CARTESIAN_POINT('Ctrl Pts',(-4.32456003949881,47.5125642776457,-48.0712916022845));
#14780=CARTESIAN_POINT('Ctrl Pts',(-4.32456003949881,47.2573567866782,-48.5139639861634));
#14781=CARTESIAN_POINT('Ctrl Pts',(-48.706329375,58.437500006828,-1.8898197019151E-14));
#14782=CARTESIAN_POINT('Ctrl Pts',(-48.706329375,58.2291666734946,-13.0508216223155));
#14783=CARTESIAN_POINT('Ctrl Pts',(-42.1809185638422,58.0208333401613,-24.3531646875));
#14784=CARTESIAN_POINT('Ctrl Pts',(-35.6555077526845,57.812500006828,-35.6555077526845));
#14785=CARTESIAN_POINT('Ctrl Pts',(-24.3531646875,57.6041666734946,-42.1809185638422));
#14786=CARTESIAN_POINT('Ctrl Pts',(-13.0508216223155,57.3958333401613,-48.706329375));
#14787=CARTESIAN_POINT('Ctrl Pts',(1.59157945007855E-14,57.187500006828,
-48.706329375));
#14788=CARTESIAN_POINT('Ctrl Pts',(13.0508216223155,56.9791666734946,-48.706329375));
#14789=CARTESIAN_POINT('Ctrl Pts',(24.3531646875,56.7708333401613,-42.1809185638422));
#14790=CARTESIAN_POINT('Ctrl Pts',(35.6555077526845,56.562500006828,-35.6555077526845));
#14791=CARTESIAN_POINT('Ctrl Pts',(42.1809185638422,56.3541666734946,-24.3531646875));
#14792=CARTESIAN_POINT('Ctrl Pts',(48.706329375,56.1458333401613,-13.0508216223155));
#14793=CARTESIAN_POINT('Ctrl Pts',(48.706329375,55.937500006828,1.293339198242E-14));
#14794=CARTESIAN_POINT('Ctrl Pts',(48.706329375,55.7291666734946,13.0508216223155));
#14795=CARTESIAN_POINT('Ctrl Pts',(42.1809185638422,55.5208333401613,24.3531646875));
#14796=CARTESIAN_POINT('Ctrl Pts',(35.6555077526845,55.312500006828,35.6555077526845));
#14797=CARTESIAN_POINT('Ctrl Pts',(24.3531646875,55.1041666734946,42.1809185638422));
#14798=CARTESIAN_POINT('Ctrl Pts',(13.0508216223155,54.8958333401613,48.706329375));
#14799=CARTESIAN_POINT('Ctrl Pts',(-9.95098946405443E-15,54.687500006828,
48.706329375));
#14800=CARTESIAN_POINT('Ctrl Pts',(-13.0508216223155,54.4791666734946,48.706329375));
#14801=CARTESIAN_POINT('Ctrl Pts',(-24.3531646875,54.2708333401613,42.1809185638423));
#14802=CARTESIAN_POINT('Ctrl Pts',(-35.6555077526845,54.062500006828,35.6555077526845));
#14803=CARTESIAN_POINT('Ctrl Pts',(-42.1809185638422,53.8541666734946,24.3531646875));
#14804=CARTESIAN_POINT('Ctrl Pts',(-48.706329375,53.6458333401613,13.0508216223155));
#14805=CARTESIAN_POINT('Ctrl Pts',(-48.706329375,53.437500006828,-1.8898197019151E-14));
#14806=CARTESIAN_POINT('Ctrl Pts',(-48.706329375,53.2291666734946,-13.0508216223155));
#14807=CARTESIAN_POINT('Ctrl Pts',(-42.1809185638422,53.0208333401613,-24.3531646875));
#14808=CARTESIAN_POINT('Ctrl Pts',(-35.6555077526845,52.812500006828,-35.6555077526845));
#14809=CARTESIAN_POINT('Ctrl Pts',(-24.3531646875,52.6041666734946,-42.1809185638422));
#14810=CARTESIAN_POINT('Ctrl Pts',(-13.0508216223155,52.3958333401613,-48.706329375));
#14811=CARTESIAN_POINT('Ctrl Pts',(1.59157945007855E-14,52.187500006828,
-48.706329375));
#14812=CARTESIAN_POINT('Ctrl Pts',(13.0508216223155,51.9791666734946,-48.706329375));
#14813=CARTESIAN_POINT('Ctrl Pts',(24.3531646875,51.7708333401613,-42.1809185638422));
#14814=CARTESIAN_POINT('Ctrl Pts',(35.6555077526845,51.562500006828,-35.6555077526845));
#14815=CARTESIAN_POINT('Ctrl Pts',(42.1809185638422,51.3541666734946,-24.3531646875));
#14816=CARTESIAN_POINT('Ctrl Pts',(48.706329375,51.1458333401613,-13.0508216223155));
#14817=CARTESIAN_POINT('Ctrl Pts',(48.706329375,50.937500006828,1.293339198242E-14));
#14818=CARTESIAN_POINT('Ctrl Pts',(48.706329375,50.7291666734946,13.0508216223155));
#14819=CARTESIAN_POINT('Ctrl Pts',(42.1809185638422,50.5208333401613,24.3531646875));
#14820=CARTESIAN_POINT('Ctrl Pts',(35.6555077526845,50.312500006828,35.6555077526845));
#14821=CARTESIAN_POINT('Ctrl Pts',(24.3531646875,50.1041666734946,42.1809185638422));
#14822=CARTESIAN_POINT('Ctrl Pts',(13.0508216223155,49.8958333401613,48.706329375));
#14823=CARTESIAN_POINT('Ctrl Pts',(-9.95098946405443E-15,49.687500006828,
48.706329375));
#14824=CARTESIAN_POINT('Ctrl Pts',(-13.0508216223155,49.4791666734946,48.706329375));
#14825=CARTESIAN_POINT('Ctrl Pts',(-24.3531646875,49.2708333401613,42.1809185638423));
#14826=CARTESIAN_POINT('Ctrl Pts',(-35.6555077526845,49.062500006828,35.6555077526845));
#14827=CARTESIAN_POINT('Ctrl Pts',(-42.1809185638422,48.8541666734946,24.3531646875));
#14828=CARTESIAN_POINT('Ctrl Pts',(-48.706329375,48.6458333401613,13.0508216223155));
#14829=CARTESIAN_POINT('Ctrl Pts',(-48.706329375,48.437500006828,-1.8898197019151E-14));
#14830=CARTESIAN_POINT('Ctrl Pts',(-48.706329375,48.2291666734946,-13.0508216223155));
#14831=CARTESIAN_POINT('Ctrl Pts',(-42.1809185638422,48.0208333401613,-24.3531646875));
#14832=CARTESIAN_POINT('Ctrl Pts',(-35.6555077526845,47.812500006828,-35.6555077526845));
#14833=CARTESIAN_POINT('Ctrl Pts',(-24.3531646875,47.6041666734946,-42.1809185638422));
#14834=CARTESIAN_POINT('Ctrl Pts',(-13.0508216223155,47.3958333401613,-48.706329375));
#14835=CARTESIAN_POINT('Ctrl Pts',(1.59157945007855E-14,47.187500006828,
-48.706329375));
#14836=CARTESIAN_POINT('Ctrl Pts',(13.0508216223155,46.9791666734946,-48.706329375));
#14837=CARTESIAN_POINT('Ctrl Pts',(24.3531646875,46.7708333401613,-42.1809185638422));
#14838=CARTESIAN_POINT('Ctrl Pts',(35.6555077526845,46.562500006828,-35.6555077526845));
#14839=CARTESIAN_POINT('Ctrl Pts',(42.1809185638422,46.3541666734946,-24.3531646875));
#14840=CARTESIAN_POINT('Ctrl Pts',(48.706329375,46.1458333401613,-13.0508216223155));
#14841=CARTESIAN_POINT('Ctrl Pts',(48.706329375,45.937500006828,1.293339198242E-14));
#14842=CARTESIAN_POINT('Ctrl Pts',(48.706329375,45.7291666734946,13.0508216223155));
#14843=CARTESIAN_POINT('Ctrl Pts',(42.1809185638422,45.5208333401613,24.3531646875));
#14844=CARTESIAN_POINT('Ctrl Pts',(35.6555077526845,45.312500006828,35.6555077526845));
#14845=CARTESIAN_POINT('Ctrl Pts',(24.3531646875,45.1041666734946,42.1809185638422));
#14846=CARTESIAN_POINT('Ctrl Pts',(13.0508216223155,44.8958333401613,48.706329375));
#14847=CARTESIAN_POINT('Ctrl Pts',(-9.95098946405443E-15,44.687500006828,
48.706329375));
#14848=CARTESIAN_POINT('Ctrl Pts',(-13.0508216223155,44.4791666734946,48.706329375));
#14849=CARTESIAN_POINT('Ctrl Pts',(-24.3531646875,44.2708333401613,42.1809185638423));
#14850=CARTESIAN_POINT('Ctrl Pts',(-35.6555077526845,44.062500006828,35.6555077526845));
#14851=CARTESIAN_POINT('Ctrl Pts',(-42.1809185638422,43.8541666734946,24.3531646875));
#14852=CARTESIAN_POINT('Ctrl Pts',(-48.706329375,43.6458333401613,13.0508216223155));
#14853=CARTESIAN_POINT('Ctrl Pts',(-48.706329375,43.437500006828,-1.8898197019151E-14));
#14854=CARTESIAN_POINT('Ctrl Pts',(-48.706329375,43.2291666734946,-13.0508216223155));
#14855=CARTESIAN_POINT('Ctrl Pts',(-42.1809185638422,43.0208333401613,-24.3531646875));
#14856=CARTESIAN_POINT('Ctrl Pts',(-35.6555077526845,42.812500006828,-35.6555077526845));
#14857=CARTESIAN_POINT('Ctrl Pts',(-24.3531646875,42.6041666734946,-42.1809185638422));
#14858=CARTESIAN_POINT('Ctrl Pts',(-13.0508216223155,42.3958333401613,-48.706329375));
#14859=CARTESIAN_POINT('Ctrl Pts',(1.59157945007855E-14,42.187500006828,
-48.706329375));
#14860=CARTESIAN_POINT('Ctrl Pts',(13.0508216223155,41.9791666734946,-48.706329375));
#14861=CARTESIAN_POINT('Ctrl Pts',(24.3531646875,41.7708333401613,-42.1809185638422));
#14862=CARTESIAN_POINT('Ctrl Pts',(35.6555077526845,41.562500006828,-35.6555077526845));
#14863=CARTESIAN_POINT('Ctrl Pts',(42.1809185638422,41.3541666734946,-24.3531646875));
#14864=CARTESIAN_POINT('Ctrl Pts',(48.706329375,41.1458333401613,-13.0508216223155));
#14865=CARTESIAN_POINT('Ctrl Pts',(48.706329375,40.937500006828,1.293339198242E-14));
#14866=CARTESIAN_POINT('Ctrl Pts',(48.706329375,40.7291666734946,13.0508216223155));
#14867=CARTESIAN_POINT('Ctrl Pts',(42.1809185638422,40.5208333401613,24.3531646875));
#14868=CARTESIAN_POINT('Ctrl Pts',(35.6555077526845,40.312500006828,35.6555077526845));
#14869=CARTESIAN_POINT('Ctrl Pts',(24.3531646875,40.1041666734946,42.1809185638422));
#14870=CARTESIAN_POINT('Ctrl Pts',(13.0508216223155,39.8958333401613,48.706329375));
#14871=CARTESIAN_POINT('Ctrl Pts',(-9.95098946405443E-15,39.687500006828,
48.706329375));
#14872=CARTESIAN_POINT('Ctrl Pts',(-13.0508216223155,39.4791666734946,48.706329375));
#14873=CARTESIAN_POINT('Ctrl Pts',(-24.3531646875,39.2708333401613,42.1809185638423));
#14874=CARTESIAN_POINT('Ctrl Pts',(-35.6555077526845,39.062500006828,35.6555077526845));
#14875=CARTESIAN_POINT('Ctrl Pts',(-42.1809185638422,38.8541666734946,24.3531646875));
#14876=CARTESIAN_POINT('Ctrl Pts',(-48.706329375,38.6458333401613,13.0508216223155));
#14877=CARTESIAN_POINT('Ctrl Pts',(-48.706329375,38.437500006828,-1.8898197019151E-14));
#14878=CARTESIAN_POINT('Ctrl Pts',(-48.706329375,38.2291666734946,-13.0508216223155));
#14879=CARTESIAN_POINT('Ctrl Pts',(-42.1809185638422,38.0208333401613,-24.3531646875));
#14880=CARTESIAN_POINT('Ctrl Pts',(-35.6555077526845,37.812500006828,-35.6555077526845));
#14881=CARTESIAN_POINT('Ctrl Pts',(-24.3531646875,37.6041666734946,-42.1809185638422));
#14882=CARTESIAN_POINT('Ctrl Pts',(-13.0508216223155,37.3958333401613,-48.706329375));
#14883=CARTESIAN_POINT('Ctrl Pts',(1.59157945007855E-14,37.187500006828,
-48.706329375));
#14884=CARTESIAN_POINT('Ctrl Pts',(13.0508216223155,36.9791666734946,-48.706329375));
#14885=CARTESIAN_POINT('Ctrl Pts',(24.3531646875,36.7708333401613,-42.1809185638422));
#14886=CARTESIAN_POINT('Ctrl Pts',(35.6555077526845,36.562500006828,-35.6555077526845));
#14887=CARTESIAN_POINT('Ctrl Pts',(42.1809185638422,36.3541666734946,-24.3531646875));
#14888=CARTESIAN_POINT('Ctrl Pts',(48.706329375,36.1458333401613,-13.0508216223155));
#14889=CARTESIAN_POINT('Ctrl Pts',(48.706329375,35.937500006828,1.293339198242E-14));
#14890=CARTESIAN_POINT('Ctrl Pts',(48.706329375,35.7291666734946,13.0508216223155));
#14891=CARTESIAN_POINT('Ctrl Pts',(42.1809185638422,35.5208333401613,24.3531646875));
#14892=CARTESIAN_POINT('Ctrl Pts',(35.6555077526845,35.312500006828,35.6555077526845));
#14893=CARTESIAN_POINT('Ctrl Pts',(24.3531646875,35.1041666734946,42.1809185638422));
#14894=CARTESIAN_POINT('Ctrl Pts',(13.0508216223155,34.8958333401613,48.706329375));
#14895=CARTESIAN_POINT('Ctrl Pts',(-9.95098946405443E-15,34.687500006828,
48.706329375));
#14896=CARTESIAN_POINT('Ctrl Pts',(-13.0508216223155,34.4791666734946,48.706329375));
#14897=CARTESIAN_POINT('Ctrl Pts',(-24.3531646875,34.2708333401613,42.1809185638423));
#14898=CARTESIAN_POINT('Ctrl Pts',(-35.6555077526845,34.062500006828,35.6555077526845));
#14899=CARTESIAN_POINT('Ctrl Pts',(-42.1809185638422,33.8541666734946,24.3531646875));
#14900=CARTESIAN_POINT('Ctrl Pts',(-48.706329375,33.6458333401613,13.0508216223155));
#14901=CARTESIAN_POINT('Ctrl Pts',(-48.706329375,33.437500006828,-1.8898197019151E-14));
#14902=CARTESIAN_POINT('Ctrl Pts',(-48.706329375,33.2291666734946,-13.0508216223155));
#14903=CARTESIAN_POINT('Ctrl Pts',(-42.1809185638422,33.0208333401613,-24.3531646875));
#14904=CARTESIAN_POINT('Ctrl Pts',(-35.6555077526845,32.812500006828,-35.6555077526845));
#14905=CARTESIAN_POINT('Ctrl Pts',(-24.3531646875,32.6041666734946,-42.1809185638422));
#14906=CARTESIAN_POINT('Ctrl Pts',(-13.0508216223155,32.3958333401613,-48.706329375));
#14907=CARTESIAN_POINT('Ctrl Pts',(1.59157945007855E-14,32.187500006828,
-48.706329375));
#14908=CARTESIAN_POINT('Ctrl Pts',(13.0508216223155,31.9791666734946,-48.706329375));
#14909=CARTESIAN_POINT('Ctrl Pts',(24.3531646875,31.7708333401613,-42.1809185638422));
#14910=CARTESIAN_POINT('Ctrl Pts',(35.6555077526845,31.562500006828,-35.6555077526845));
#14911=CARTESIAN_POINT('Ctrl Pts',(42.1809185638422,31.3541666734946,-24.3531646875));
#14912=CARTESIAN_POINT('Ctrl Pts',(48.706329375,31.1458333401613,-13.0508216223155));
#14913=CARTESIAN_POINT('Ctrl Pts',(48.706329375,30.937500006828,1.293339198242E-14));
#14914=CARTESIAN_POINT('Ctrl Pts',(48.706329375,30.7291666734946,13.0508216223155));
#14915=CARTESIAN_POINT('Ctrl Pts',(42.1809185638422,30.5208333401613,24.3531646875));
#14916=CARTESIAN_POINT('Ctrl Pts',(35.6555077526845,30.312500006828,35.6555077526845));
#14917=CARTESIAN_POINT('Ctrl Pts',(24.3531646875,30.1041666734946,42.1809185638422));
#14918=CARTESIAN_POINT('Ctrl Pts',(13.0508216223155,29.8958333401613,48.706329375));
#14919=CARTESIAN_POINT('Ctrl Pts',(-9.95098946405443E-15,29.687500006828,
48.706329375));
#14920=CARTESIAN_POINT('Ctrl Pts',(-13.0508216223155,29.4791666734946,48.706329375));
#14921=CARTESIAN_POINT('Ctrl Pts',(-24.3531646875,29.2708333401613,42.1809185638423));
#14922=CARTESIAN_POINT('Ctrl Pts',(-35.6555077526845,29.062500006828,35.6555077526845));
#14923=CARTESIAN_POINT('Ctrl Pts',(-42.1809185638422,28.8541666734946,24.3531646875));
#14924=CARTESIAN_POINT('Ctrl Pts',(-48.706329375,28.6458333401613,13.0508216223155));
#14925=CARTESIAN_POINT('Ctrl Pts',(-48.706329375,28.437500006828,-1.8898197019151E-14));
#14926=CARTESIAN_POINT('Ctrl Pts',(-46.,60.,0.));
#14927=CARTESIAN_POINT('Ctrl Pts',(-46.,59.7916666666667,-12.3256628518316));
#14928=CARTESIAN_POINT('Ctrl Pts',(-39.8371685740842,59.5833333333333,-23.));
#14929=CARTESIAN_POINT('Ctrl Pts',(-33.6743371481684,59.375,-33.6743371481684));
#14930=CARTESIAN_POINT('Ctrl Pts',(-23.,59.1666666666667,-39.8371685740842));
#14931=CARTESIAN_POINT('Ctrl Pts',(-12.3256628518317,58.9583333333333,-46.));
#14932=CARTESIAN_POINT('Ctrl Pts',(-2.81668763803891E-15,58.75,-46.));
#14933=CARTESIAN_POINT('Ctrl Pts',(12.3256628518316,58.5416666666667,-46.));
#14934=CARTESIAN_POINT('Ctrl Pts',(23.,58.3333333333333,-39.8371685740842));
#14935=CARTESIAN_POINT('Ctrl Pts',(33.6743371481683,58.125,-33.6743371481684));
#14936=CARTESIAN_POINT('Ctrl Pts',(39.8371685740842,57.9166666666667,-23.));
#14937=CARTESIAN_POINT('Ctrl Pts',(46.,57.7083333333333,-12.3256628518317));
#14938=CARTESIAN_POINT('Ctrl Pts',(46.,57.5,-5.63337527607782E-15));
#14939=CARTESIAN_POINT('Ctrl Pts',(46.,57.2916666666667,12.3256628518316));
#14940=CARTESIAN_POINT('Ctrl Pts',(39.8371685740842,57.0833333333333,23.));
#14941=CARTESIAN_POINT('Ctrl Pts',(33.6743371481684,56.875,33.6743371481683));
#14942=CARTESIAN_POINT('Ctrl Pts',(23.,56.6666666666667,39.8371685740842));
#14943=CARTESIAN_POINT('Ctrl Pts',(12.3256628518317,56.4583333333333,46.));
#14944=CARTESIAN_POINT('Ctrl Pts',(8.45006291411674E-15,56.25,46.));
#14945=CARTESIAN_POINT('Ctrl Pts',(-12.3256628518316,56.0416666666667,46.));
#14946=CARTESIAN_POINT('Ctrl Pts',(-23.,55.8333333333333,39.8371685740842));
#14947=CARTESIAN_POINT('Ctrl Pts',(-33.6743371481683,55.625,33.6743371481684));
#14948=CARTESIAN_POINT('Ctrl Pts',(-39.8371685740842,55.4166666666667,23.));
#14949=CARTESIAN_POINT('Ctrl Pts',(-46.,55.2083333333333,12.3256628518317));
#14950=CARTESIAN_POINT('Ctrl Pts',(-46.,55.,0.));
#14951=CARTESIAN_POINT('Ctrl Pts',(-46.,54.7916666666667,-12.3256628518316));
#14952=CARTESIAN_POINT('Ctrl Pts',(-39.8371685740842,54.5833333333333,-23.));
#14953=CARTESIAN_POINT('Ctrl Pts',(-33.6743371481684,54.375,-33.6743371481684));
#14954=CARTESIAN_POINT('Ctrl Pts',(-23.,54.1666666666667,-39.8371685740842));
#14955=CARTESIAN_POINT('Ctrl Pts',(-12.3256628518317,53.9583333333333,-46.));
#14956=CARTESIAN_POINT('Ctrl Pts',(-2.81668763803891E-15,53.75,-46.));
#14957=CARTESIAN_POINT('Ctrl Pts',(12.3256628518316,53.5416666666667,-46.));
#14958=CARTESIAN_POINT('Ctrl Pts',(23.,53.3333333333333,-39.8371685740842));
#14959=CARTESIAN_POINT('Ctrl Pts',(33.6743371481683,53.125,-33.6743371481684));
#14960=CARTESIAN_POINT('Ctrl Pts',(39.8371685740842,52.9166666666667,-23.));
#14961=CARTESIAN_POINT('Ctrl Pts',(46.,52.7083333333333,-12.3256628518317));
#14962=CARTESIAN_POINT('Ctrl Pts',(46.,52.5,-5.63337527607782E-15));
#14963=CARTESIAN_POINT('Ctrl Pts',(46.,52.2916666666667,12.3256628518316));
#14964=CARTESIAN_POINT('Ctrl Pts',(39.8371685740842,52.0833333333333,23.));
#14965=CARTESIAN_POINT('Ctrl Pts',(33.6743371481684,51.875,33.6743371481683));
#14966=CARTESIAN_POINT('Ctrl Pts',(23.,51.6666666666667,39.8371685740842));
#14967=CARTESIAN_POINT('Ctrl Pts',(12.3256628518317,51.4583333333333,46.));
#14968=CARTESIAN_POINT('Ctrl Pts',(8.45006291411674E-15,51.25,46.));
#14969=CARTESIAN_POINT('Ctrl Pts',(-12.3256628518316,51.0416666666667,46.));
#14970=CARTESIAN_POINT('Ctrl Pts',(-23.,50.8333333333333,39.8371685740842));
#14971=CARTESIAN_POINT('Ctrl Pts',(-33.6743371481683,50.625,33.6743371481684));
#14972=CARTESIAN_POINT('Ctrl Pts',(-39.8371685740842,50.4166666666667,23.));
#14973=CARTESIAN_POINT('Ctrl Pts',(-46.,50.2083333333333,12.3256628518317));
#14974=CARTESIAN_POINT('Ctrl Pts',(-46.,50.,0.));
#14975=CARTESIAN_POINT('Ctrl Pts',(-46.,49.7916666666667,-12.3256628518316));
#14976=CARTESIAN_POINT('Ctrl Pts',(-39.8371685740842,49.5833333333333,-23.));
#14977=CARTESIAN_POINT('Ctrl Pts',(-33.6743371481684,49.375,-33.6743371481684));
#14978=CARTESIAN_POINT('Ctrl Pts',(-23.,49.1666666666667,-39.8371685740842));
#14979=CARTESIAN_POINT('Ctrl Pts',(-12.3256628518317,48.9583333333333,-46.));
#14980=CARTESIAN_POINT('Ctrl Pts',(-2.81668763803891E-15,48.75,-46.));
#14981=CARTESIAN_POINT('Ctrl Pts',(12.3256628518316,48.5416666666667,-46.));
#14982=CARTESIAN_POINT('Ctrl Pts',(23.,48.3333333333333,-39.8371685740842));
#14983=CARTESIAN_POINT('Ctrl Pts',(33.6743371481683,48.125,-33.6743371481684));
#14984=CARTESIAN_POINT('Ctrl Pts',(39.8371685740842,47.9166666666667,-23.));
#14985=CARTESIAN_POINT('Ctrl Pts',(46.,47.7083333333333,-12.3256628518317));
#14986=CARTESIAN_POINT('Ctrl Pts',(46.,47.5,-5.63337527607782E-15));
#14987=CARTESIAN_POINT('Ctrl Pts',(46.,47.2916666666667,12.3256628518316));
#14988=CARTESIAN_POINT('Ctrl Pts',(39.8371685740842,47.0833333333333,23.));
#14989=CARTESIAN_POINT('Ctrl Pts',(33.6743371481684,46.875,33.6743371481683));
#14990=CARTESIAN_POINT('Ctrl Pts',(23.,46.6666666666667,39.8371685740842));
#14991=CARTESIAN_POINT('Ctrl Pts',(12.3256628518317,46.4583333333333,46.));
#14992=CARTESIAN_POINT('Ctrl Pts',(8.45006291411674E-15,46.25,46.));
#14993=CARTESIAN_POINT('Ctrl Pts',(-12.3256628518316,46.0416666666667,46.));
#14994=CARTESIAN_POINT('Ctrl Pts',(-23.,45.8333333333333,39.8371685740842));
#14995=CARTESIAN_POINT('Ctrl Pts',(-33.6743371481683,45.625,33.6743371481684));
#14996=CARTESIAN_POINT('Ctrl Pts',(-39.8371685740842,45.4166666666667,23.));
#14997=CARTESIAN_POINT('Ctrl Pts',(-46.,45.2083333333333,12.3256628518317));
#14998=CARTESIAN_POINT('Ctrl Pts',(-46.,45.,0.));
#14999=CARTESIAN_POINT('Ctrl Pts',(-46.,44.7916666666667,-12.3256628518316));
#15000=CARTESIAN_POINT('Ctrl Pts',(-39.8371685740842,44.5833333333333,-23.));
#15001=CARTESIAN_POINT('Ctrl Pts',(-33.6743371481684,44.375,-33.6743371481684));
#15002=CARTESIAN_POINT('Ctrl Pts',(-23.,44.1666666666667,-39.8371685740842));
#15003=CARTESIAN_POINT('Ctrl Pts',(-12.3256628518317,43.9583333333333,-46.));
#15004=CARTESIAN_POINT('Ctrl Pts',(-2.81668763803891E-15,43.75,-46.));
#15005=CARTESIAN_POINT('Ctrl Pts',(12.3256628518316,43.5416666666667,-46.));
#15006=CARTESIAN_POINT('Ctrl Pts',(23.,43.3333333333333,-39.8371685740842));
#15007=CARTESIAN_POINT('Ctrl Pts',(33.6743371481683,43.125,-33.6743371481684));
#15008=CARTESIAN_POINT('Ctrl Pts',(39.8371685740842,42.9166666666667,-23.));
#15009=CARTESIAN_POINT('Ctrl Pts',(46.,42.7083333333333,-12.3256628518317));
#15010=CARTESIAN_POINT('Ctrl Pts',(46.,42.5,-5.63337527607782E-15));
#15011=CARTESIAN_POINT('Ctrl Pts',(46.,42.2916666666667,12.3256628518316));
#15012=CARTESIAN_POINT('Ctrl Pts',(39.8371685740842,42.0833333333333,23.));
#15013=CARTESIAN_POINT('Ctrl Pts',(33.6743371481684,41.875,33.6743371481683));
#15014=CARTESIAN_POINT('Ctrl Pts',(23.,41.6666666666667,39.8371685740842));
#15015=CARTESIAN_POINT('Ctrl Pts',(12.3256628518317,41.4583333333333,46.));
#15016=CARTESIAN_POINT('Ctrl Pts',(8.45006291411674E-15,41.25,46.));
#15017=CARTESIAN_POINT('Ctrl Pts',(-12.3256628518316,41.0416666666667,46.));
#15018=CARTESIAN_POINT('Ctrl Pts',(-23.,40.8333333333333,39.8371685740842));
#15019=CARTESIAN_POINT('Ctrl Pts',(-33.6743371481683,40.625,33.6743371481684));
#15020=CARTESIAN_POINT('Ctrl Pts',(-39.8371685740842,40.4166666666667,23.));
#15021=CARTESIAN_POINT('Ctrl Pts',(-46.,40.2083333333333,12.3256628518317));
#15022=CARTESIAN_POINT('Ctrl Pts',(-46.,40.,0.));
#15023=CARTESIAN_POINT('Ctrl Pts',(-46.,39.7916666666667,-12.3256628518316));
#15024=CARTESIAN_POINT('Ctrl Pts',(-39.8371685740842,39.5833333333333,-23.));
#15025=CARTESIAN_POINT('Ctrl Pts',(-33.6743371481684,39.375,-33.6743371481684));
#15026=CARTESIAN_POINT('Ctrl Pts',(-23.,39.1666666666667,-39.8371685740842));
#15027=CARTESIAN_POINT('Ctrl Pts',(-12.3256628518317,38.9583333333333,-46.));
#15028=CARTESIAN_POINT('Ctrl Pts',(-2.81668763803891E-15,38.75,-46.));
#15029=CARTESIAN_POINT('Ctrl Pts',(12.3256628518316,38.5416666666667,-46.));
#15030=CARTESIAN_POINT('Ctrl Pts',(23.,38.3333333333333,-39.8371685740842));
#15031=CARTESIAN_POINT('Ctrl Pts',(33.6743371481683,38.125,-33.6743371481684));
#15032=CARTESIAN_POINT('Ctrl Pts',(39.8371685740842,37.9166666666667,-23.));
#15033=CARTESIAN_POINT('Ctrl Pts',(46.,37.7083333333333,-12.3256628518317));
#15034=CARTESIAN_POINT('Ctrl Pts',(46.,37.5,-5.63337527607782E-15));
#15035=CARTESIAN_POINT('Ctrl Pts',(46.,37.2916666666667,12.3256628518316));
#15036=CARTESIAN_POINT('Ctrl Pts',(39.8371685740842,37.0833333333333,23.));
#15037=CARTESIAN_POINT('Ctrl Pts',(33.6743371481684,36.875,33.6743371481683));
#15038=CARTESIAN_POINT('Ctrl Pts',(23.,36.6666666666667,39.8371685740842));
#15039=CARTESIAN_POINT('Ctrl Pts',(12.3256628518317,36.4583333333333,46.));
#15040=CARTESIAN_POINT('Ctrl Pts',(8.45006291411674E-15,36.25,46.));
#15041=CARTESIAN_POINT('Ctrl Pts',(-12.3256628518316,36.0416666666667,46.));
#15042=CARTESIAN_POINT('Ctrl Pts',(-23.,35.8333333333333,39.8371685740842));
#15043=CARTESIAN_POINT('Ctrl Pts',(-33.6743371481683,35.625,33.6743371481684));
#15044=CARTESIAN_POINT('Ctrl Pts',(-39.8371685740842,35.4166666666667,23.));
#15045=CARTESIAN_POINT('Ctrl Pts',(-46.,35.2083333333333,12.3256628518317));
#15046=CARTESIAN_POINT('Ctrl Pts',(-46.,35.,0.));
#15047=CARTESIAN_POINT('Ctrl Pts',(-46.,34.7916666666667,-12.3256628518316));
#15048=CARTESIAN_POINT('Ctrl Pts',(-39.8371685740842,34.5833333333333,-23.));
#15049=CARTESIAN_POINT('Ctrl Pts',(-33.6743371481684,34.375,-33.6743371481684));
#15050=CARTESIAN_POINT('Ctrl Pts',(-23.,34.1666666666667,-39.8371685740842));
#15051=CARTESIAN_POINT('Ctrl Pts',(-12.3256628518317,33.9583333333333,-46.));
#15052=CARTESIAN_POINT('Ctrl Pts',(-2.81668763803891E-15,33.75,-46.));
#15053=CARTESIAN_POINT('Ctrl Pts',(12.3256628518316,33.5416666666667,-46.));
#15054=CARTESIAN_POINT('Ctrl Pts',(23.,33.3333333333333,-39.8371685740842));
#15055=CARTESIAN_POINT('Ctrl Pts',(33.6743371481683,33.125,-33.6743371481684));
#15056=CARTESIAN_POINT('Ctrl Pts',(39.8371685740842,32.9166666666667,-23.));
#15057=CARTESIAN_POINT('Ctrl Pts',(46.,32.7083333333333,-12.3256628518317));
#15058=CARTESIAN_POINT('Ctrl Pts',(46.,32.5,-5.63337527607782E-15));
#15059=CARTESIAN_POINT('Ctrl Pts',(46.,32.2916666666667,12.3256628518316));
#15060=CARTESIAN_POINT('Ctrl Pts',(39.8371685740842,32.0833333333333,23.));
#15061=CARTESIAN_POINT('Ctrl Pts',(33.6743371481684,31.875,33.6743371481683));
#15062=CARTESIAN_POINT('Ctrl Pts',(23.,31.6666666666667,39.8371685740842));
#15063=CARTESIAN_POINT('Ctrl Pts',(12.3256628518317,31.4583333333333,46.));
#15064=CARTESIAN_POINT('Ctrl Pts',(8.45006291411674E-15,31.25,46.));
#15065=CARTESIAN_POINT('Ctrl Pts',(-12.3256628518316,31.0416666666667,46.));
#15066=CARTESIAN_POINT('Ctrl Pts',(-23.,30.8333333333333,39.8371685740842));
#15067=CARTESIAN_POINT('Ctrl Pts',(-33.6743371481683,30.625,33.6743371481684));
#15068=CARTESIAN_POINT('Ctrl Pts',(-39.8371685740842,30.4166666666667,23.));
#15069=CARTESIAN_POINT('Ctrl Pts',(-46.,30.2083333333333,12.3256628518317));
#15070=CARTESIAN_POINT('Ctrl Pts',(-46.,30.,0.));
#15071=CARTESIAN_POINT('Ctrl Pts',(-45.858362923034,50.061608680256,3.60701400320326));
#15072=CARTESIAN_POINT('Ctrl Pts',(-46.089925771934,49.9280150456296,3.60701400320326));
#15073=CARTESIAN_POINT('Ctrl Pts',(-46.5530501979845,49.6608255719955,3.60701400320326));
#15074=CARTESIAN_POINT('Ctrl Pts',(-47.0161721905706,49.3936318804496,3.60701400320324));
#15075=CARTESIAN_POINT('Ctrl Pts',(-47.6893519862319,49.0052434879083,3.60701400320324));
#15076=CARTESIAN_POINT('Ctrl Pts',(-48.1309692507095,48.7504492807381,3.60701400320326));
#15077=CARTESIAN_POINT('Ctrl Pts',(-48.5725845633798,48.4956516907297,3.60701400320326));
#15078=CARTESIAN_POINT('Origin',(-4.32456000128674,-7921.57954027603,-4524.01087374411));
#15079=CARTESIAN_POINT('Ctrl Pts',(-48.706329375,58.437500006828,-1.8898197019151E-14));
#15080=CARTESIAN_POINT('Ctrl Pts',(-48.706329375,58.2291666734946,-13.0508216223155));
#15081=CARTESIAN_POINT('Ctrl Pts',(-42.1809185638422,58.0208333401613,-24.3531646875));
#15082=CARTESIAN_POINT('Ctrl Pts',(-35.6555077526845,57.812500006828,-35.6555077526845));
#15083=CARTESIAN_POINT('Ctrl Pts',(-24.3531646875,57.6041666734946,-42.1809185638422));
#15084=CARTESIAN_POINT('Ctrl Pts',(-13.0508216223155,57.3958333401613,-48.706329375));
#15085=CARTESIAN_POINT('Ctrl Pts',(1.59157945007855E-14,57.187500006828,
-48.706329375));
#15086=CARTESIAN_POINT('Ctrl Pts',(13.0508216223155,56.9791666734946,-48.706329375));
#15087=CARTESIAN_POINT('Ctrl Pts',(24.3531646875,56.7708333401613,-42.1809185638422));
#15088=CARTESIAN_POINT('Ctrl Pts',(35.6555077526845,56.562500006828,-35.6555077526845));
#15089=CARTESIAN_POINT('Ctrl Pts',(42.1809185638422,56.3541666734946,-24.3531646875));
#15090=CARTESIAN_POINT('Ctrl Pts',(48.706329375,56.1458333401613,-13.0508216223155));
#15091=CARTESIAN_POINT('Ctrl Pts',(48.706329375,55.937500006828,1.293339198242E-14));
#15092=CARTESIAN_POINT('Ctrl Pts',(48.706329375,55.7291666734946,13.0508216223155));
#15093=CARTESIAN_POINT('Ctrl Pts',(42.1809185638422,55.5208333401613,24.3531646875));
#15094=CARTESIAN_POINT('Ctrl Pts',(35.6555077526845,55.312500006828,35.6555077526845));
#15095=CARTESIAN_POINT('Ctrl Pts',(24.3531646875,55.1041666734946,42.1809185638422));
#15096=CARTESIAN_POINT('Ctrl Pts',(13.0508216223155,54.8958333401613,48.706329375));
#15097=CARTESIAN_POINT('Ctrl Pts',(-9.95098946405443E-15,54.687500006828,
48.706329375));
#15098=CARTESIAN_POINT('Ctrl Pts',(-13.0508216223155,54.4791666734946,48.706329375));
#15099=CARTESIAN_POINT('Ctrl Pts',(-24.3531646875,54.2708333401613,42.1809185638423));
#15100=CARTESIAN_POINT('Ctrl Pts',(-35.6555077526845,54.062500006828,35.6555077526845));
#15101=CARTESIAN_POINT('Ctrl Pts',(-42.1809185638422,53.8541666734946,24.3531646875));
#15102=CARTESIAN_POINT('Ctrl Pts',(-48.706329375,53.6458333401613,13.0508216223155));
#15103=CARTESIAN_POINT('Ctrl Pts',(-48.706329375,53.437500006828,-1.8898197019151E-14));
#15104=CARTESIAN_POINT('Ctrl Pts',(-48.706329375,53.2291666734946,-13.0508216223155));
#15105=CARTESIAN_POINT('Ctrl Pts',(-42.1809185638422,53.0208333401613,-24.3531646875));
#15106=CARTESIAN_POINT('Ctrl Pts',(-35.6555077526845,52.812500006828,-35.6555077526845));
#15107=CARTESIAN_POINT('Ctrl Pts',(-24.3531646875,52.6041666734946,-42.1809185638422));
#15108=CARTESIAN_POINT('Ctrl Pts',(-13.0508216223155,52.3958333401613,-48.706329375));
#15109=CARTESIAN_POINT('Ctrl Pts',(1.59157945007855E-14,52.187500006828,
-48.706329375));
#15110=CARTESIAN_POINT('Ctrl Pts',(13.0508216223155,51.9791666734946,-48.706329375));
#15111=CARTESIAN_POINT('Ctrl Pts',(24.3531646875,51.7708333401613,-42.1809185638422));
#15112=CARTESIAN_POINT('Ctrl Pts',(35.6555077526845,51.562500006828,-35.6555077526845));
#15113=CARTESIAN_POINT('Ctrl Pts',(42.1809185638422,51.3541666734946,-24.3531646875));
#15114=CARTESIAN_POINT('Ctrl Pts',(48.706329375,51.1458333401613,-13.0508216223155));
#15115=CARTESIAN_POINT('Ctrl Pts',(48.706329375,50.937500006828,1.293339198242E-14));
#15116=CARTESIAN_POINT('Ctrl Pts',(48.706329375,50.7291666734946,13.0508216223155));
#15117=CARTESIAN_POINT('Ctrl Pts',(42.1809185638422,50.5208333401613,24.3531646875));
#15118=CARTESIAN_POINT('Ctrl Pts',(35.6555077526845,50.312500006828,35.6555077526845));
#15119=CARTESIAN_POINT('Ctrl Pts',(24.3531646875,50.1041666734946,42.1809185638422));
#15120=CARTESIAN_POINT('Ctrl Pts',(13.0508216223155,49.8958333401613,48.706329375));
#15121=CARTESIAN_POINT('Ctrl Pts',(-9.95098946405443E-15,49.687500006828,
48.706329375));
#15122=CARTESIAN_POINT('Ctrl Pts',(-13.0508216223155,49.4791666734946,48.706329375));
#15123=CARTESIAN_POINT('Ctrl Pts',(-24.3531646875,49.2708333401613,42.1809185638423));
#15124=CARTESIAN_POINT('Ctrl Pts',(-35.6555077526845,49.062500006828,35.6555077526845));
#15125=CARTESIAN_POINT('Ctrl Pts',(-42.1809185638422,48.8541666734946,24.3531646875));
#15126=CARTESIAN_POINT('Ctrl Pts',(-48.706329375,48.6458333401613,13.0508216223155));
#15127=CARTESIAN_POINT('Ctrl Pts',(-48.706329375,48.437500006828,-1.8898197019151E-14));
#15128=CARTESIAN_POINT('Ctrl Pts',(-48.706329375,48.2291666734946,-13.0508216223155));
#15129=CARTESIAN_POINT('Ctrl Pts',(-42.1809185638422,48.0208333401613,-24.3531646875));
#15130=CARTESIAN_POINT('Ctrl Pts',(-35.6555077526845,47.812500006828,-35.6555077526845));
#15131=CARTESIAN_POINT('Ctrl Pts',(-24.3531646875,47.6041666734946,-42.1809185638422));
#15132=CARTESIAN_POINT('Ctrl Pts',(-13.0508216223155,47.3958333401613,-48.706329375));
#15133=CARTESIAN_POINT('Ctrl Pts',(1.59157945007855E-14,47.187500006828,
-48.706329375));
#15134=CARTESIAN_POINT('Ctrl Pts',(13.0508216223155,46.9791666734946,-48.706329375));
#15135=CARTESIAN_POINT('Ctrl Pts',(24.3531646875,46.7708333401613,-42.1809185638422));
#15136=CARTESIAN_POINT('Ctrl Pts',(35.6555077526845,46.562500006828,-35.6555077526845));
#15137=CARTESIAN_POINT('Ctrl Pts',(42.1809185638422,46.3541666734946,-24.3531646875));
#15138=CARTESIAN_POINT('Ctrl Pts',(48.706329375,46.1458333401613,-13.0508216223155));
#15139=CARTESIAN_POINT('Ctrl Pts',(48.706329375,45.937500006828,1.293339198242E-14));
#15140=CARTESIAN_POINT('Ctrl Pts',(48.706329375,45.7291666734946,13.0508216223155));
#15141=CARTESIAN_POINT('Ctrl Pts',(42.1809185638422,45.5208333401613,24.3531646875));
#15142=CARTESIAN_POINT('Ctrl Pts',(35.6555077526845,45.312500006828,35.6555077526845));
#15143=CARTESIAN_POINT('Ctrl Pts',(24.3531646875,45.1041666734946,42.1809185638422));
#15144=CARTESIAN_POINT('Ctrl Pts',(13.0508216223155,44.8958333401613,48.706329375));
#15145=CARTESIAN_POINT('Ctrl Pts',(-9.95098946405443E-15,44.687500006828,
48.706329375));
#15146=CARTESIAN_POINT('Ctrl Pts',(-13.0508216223155,44.4791666734946,48.706329375));
#15147=CARTESIAN_POINT('Ctrl Pts',(-24.3531646875,44.2708333401613,42.1809185638423));
#15148=CARTESIAN_POINT('Ctrl Pts',(-35.6555077526845,44.062500006828,35.6555077526845));
#15149=CARTESIAN_POINT('Ctrl Pts',(-42.1809185638422,43.8541666734946,24.3531646875));
#15150=CARTESIAN_POINT('Ctrl Pts',(-48.706329375,43.6458333401613,13.0508216223155));
#15151=CARTESIAN_POINT('Ctrl Pts',(-48.706329375,43.437500006828,-1.8898197019151E-14));
#15152=CARTESIAN_POINT('Ctrl Pts',(-48.706329375,43.2291666734946,-13.0508216223155));
#15153=CARTESIAN_POINT('Ctrl Pts',(-42.1809185638422,43.0208333401613,-24.3531646875));
#15154=CARTESIAN_POINT('Ctrl Pts',(-35.6555077526845,42.812500006828,-35.6555077526845));
#15155=CARTESIAN_POINT('Ctrl Pts',(-24.3531646875,42.6041666734946,-42.1809185638422));
#15156=CARTESIAN_POINT('Ctrl Pts',(-13.0508216223155,42.3958333401613,-48.706329375));
#15157=CARTESIAN_POINT('Ctrl Pts',(1.59157945007855E-14,42.187500006828,
-48.706329375));
#15158=CARTESIAN_POINT('Ctrl Pts',(13.0508216223155,41.9791666734946,-48.706329375));
#15159=CARTESIAN_POINT('Ctrl Pts',(24.3531646875,41.7708333401613,-42.1809185638422));
#15160=CARTESIAN_POINT('Ctrl Pts',(35.6555077526845,41.562500006828,-35.6555077526845));
#15161=CARTESIAN_POINT('Ctrl Pts',(42.1809185638422,41.3541666734946,-24.3531646875));
#15162=CARTESIAN_POINT('Ctrl Pts',(48.706329375,41.1458333401613,-13.0508216223155));
#15163=CARTESIAN_POINT('Ctrl Pts',(48.706329375,40.937500006828,1.293339198242E-14));
#15164=CARTESIAN_POINT('Ctrl Pts',(48.706329375,40.7291666734946,13.0508216223155));
#15165=CARTESIAN_POINT('Ctrl Pts',(42.1809185638422,40.5208333401613,24.3531646875));
#15166=CARTESIAN_POINT('Ctrl Pts',(35.6555077526845,40.312500006828,35.6555077526845));
#15167=CARTESIAN_POINT('Ctrl Pts',(24.3531646875,40.1041666734946,42.1809185638422));
#15168=CARTESIAN_POINT('Ctrl Pts',(13.0508216223155,39.8958333401613,48.706329375));
#15169=CARTESIAN_POINT('Ctrl Pts',(-9.95098946405443E-15,39.687500006828,
48.706329375));
#15170=CARTESIAN_POINT('Ctrl Pts',(-13.0508216223155,39.4791666734946,48.706329375));
#15171=CARTESIAN_POINT('Ctrl Pts',(-24.3531646875,39.2708333401613,42.1809185638423));
#15172=CARTESIAN_POINT('Ctrl Pts',(-35.6555077526845,39.062500006828,35.6555077526845));
#15173=CARTESIAN_POINT('Ctrl Pts',(-42.1809185638422,38.8541666734946,24.3531646875));
#15174=CARTESIAN_POINT('Ctrl Pts',(-48.706329375,38.6458333401613,13.0508216223155));
#15175=CARTESIAN_POINT('Ctrl Pts',(-48.706329375,38.437500006828,-1.8898197019151E-14));
#15176=CARTESIAN_POINT('Ctrl Pts',(-48.706329375,38.2291666734946,-13.0508216223155));
#15177=CARTESIAN_POINT('Ctrl Pts',(-42.1809185638422,38.0208333401613,-24.3531646875));
#15178=CARTESIAN_POINT('Ctrl Pts',(-35.6555077526845,37.812500006828,-35.6555077526845));
#15179=CARTESIAN_POINT('Ctrl Pts',(-24.3531646875,37.6041666734946,-42.1809185638422));
#15180=CARTESIAN_POINT('Ctrl Pts',(-13.0508216223155,37.3958333401613,-48.706329375));
#15181=CARTESIAN_POINT('Ctrl Pts',(1.59157945007855E-14,37.187500006828,
-48.706329375));
#15182=CARTESIAN_POINT('Ctrl Pts',(13.0508216223155,36.9791666734946,-48.706329375));
#15183=CARTESIAN_POINT('Ctrl Pts',(24.3531646875,36.7708333401613,-42.1809185638422));
#15184=CARTESIAN_POINT('Ctrl Pts',(35.6555077526845,36.562500006828,-35.6555077526845));
#15185=CARTESIAN_POINT('Ctrl Pts',(42.1809185638422,36.3541666734946,-24.3531646875));
#15186=CARTESIAN_POINT('Ctrl Pts',(48.706329375,36.1458333401613,-13.0508216223155));
#15187=CARTESIAN_POINT('Ctrl Pts',(48.706329375,35.937500006828,1.293339198242E-14));
#15188=CARTESIAN_POINT('Ctrl Pts',(48.706329375,35.7291666734946,13.0508216223155));
#15189=CARTESIAN_POINT('Ctrl Pts',(42.1809185638422,35.5208333401613,24.3531646875));
#15190=CARTESIAN_POINT('Ctrl Pts',(35.6555077526845,35.312500006828,35.6555077526845));
#15191=CARTESIAN_POINT('Ctrl Pts',(24.3531646875,35.1041666734946,42.1809185638422));
#15192=CARTESIAN_POINT('Ctrl Pts',(13.0508216223155,34.8958333401613,48.706329375));
#15193=CARTESIAN_POINT('Ctrl Pts',(-9.95098946405443E-15,34.687500006828,
48.706329375));
#15194=CARTESIAN_POINT('Ctrl Pts',(-13.0508216223155,34.4791666734946,48.706329375));
#15195=CARTESIAN_POINT('Ctrl Pts',(-24.3531646875,34.2708333401613,42.1809185638423));
#15196=CARTESIAN_POINT('Ctrl Pts',(-35.6555077526845,34.062500006828,35.6555077526845));
#15197=CARTESIAN_POINT('Ctrl Pts',(-42.1809185638422,33.8541666734946,24.3531646875));
#15198=CARTESIAN_POINT('Ctrl Pts',(-48.706329375,33.6458333401613,13.0508216223155));
#15199=CARTESIAN_POINT('Ctrl Pts',(-48.706329375,33.437500006828,-1.8898197019151E-14));
#15200=CARTESIAN_POINT('Ctrl Pts',(-48.706329375,33.2291666734946,-13.0508216223155));
#15201=CARTESIAN_POINT('Ctrl Pts',(-42.1809185638422,33.0208333401613,-24.3531646875));
#15202=CARTESIAN_POINT('Ctrl Pts',(-35.6555077526845,32.812500006828,-35.6555077526845));
#15203=CARTESIAN_POINT('Ctrl Pts',(-24.3531646875,32.6041666734946,-42.1809185638422));
#15204=CARTESIAN_POINT('Ctrl Pts',(-13.0508216223155,32.3958333401613,-48.706329375));
#15205=CARTESIAN_POINT('Ctrl Pts',(1.59157945007855E-14,32.187500006828,
-48.706329375));
#15206=CARTESIAN_POINT('Ctrl Pts',(13.0508216223155,31.9791666734946,-48.706329375));
#15207=CARTESIAN_POINT('Ctrl Pts',(24.3531646875,31.7708333401613,-42.1809185638422));
#15208=CARTESIAN_POINT('Ctrl Pts',(35.6555077526845,31.562500006828,-35.6555077526845));
#15209=CARTESIAN_POINT('Ctrl Pts',(42.1809185638422,31.3541666734946,-24.3531646875));
#15210=CARTESIAN_POINT('Ctrl Pts',(48.706329375,31.1458333401613,-13.0508216223155));
#15211=CARTESIAN_POINT('Ctrl Pts',(48.706329375,30.937500006828,1.293339198242E-14));
#15212=CARTESIAN_POINT('Ctrl Pts',(48.706329375,30.7291666734946,13.0508216223155));
#15213=CARTESIAN_POINT('Ctrl Pts',(42.1809185638422,30.5208333401613,24.3531646875));
#15214=CARTESIAN_POINT('Ctrl Pts',(35.6555077526845,30.312500006828,35.6555077526845));
#15215=CARTESIAN_POINT('Ctrl Pts',(24.3531646875,30.1041666734946,42.1809185638422));
#15216=CARTESIAN_POINT('Ctrl Pts',(13.0508216223155,29.8958333401613,48.706329375));
#15217=CARTESIAN_POINT('Ctrl Pts',(-9.95098946405443E-15,29.687500006828,
48.706329375));
#15218=CARTESIAN_POINT('Ctrl Pts',(-13.0508216223155,29.4791666734946,48.706329375));
#15219=CARTESIAN_POINT('Ctrl Pts',(-24.3531646875,29.2708333401613,42.1809185638423));
#15220=CARTESIAN_POINT('Ctrl Pts',(-35.6555077526845,29.062500006828,35.6555077526845));
#15221=CARTESIAN_POINT('Ctrl Pts',(-42.1809185638422,28.8541666734946,24.3531646875));
#15222=CARTESIAN_POINT('Ctrl Pts',(-48.706329375,28.6458333401613,13.0508216223155));
#15223=CARTESIAN_POINT('Ctrl Pts',(-48.706329375,28.437500006828,-1.8898197019151E-14));
#15224=CARTESIAN_POINT('Ctrl Pts',(-46.,60.,0.));
#15225=CARTESIAN_POINT('Ctrl Pts',(-46.,59.7916666666667,-12.3256628518316));
#15226=CARTESIAN_POINT('Ctrl Pts',(-39.8371685740842,59.5833333333333,-23.));
#15227=CARTESIAN_POINT('Ctrl Pts',(-33.6743371481684,59.375,-33.6743371481684));
#15228=CARTESIAN_POINT('Ctrl Pts',(-23.,59.1666666666667,-39.8371685740842));
#15229=CARTESIAN_POINT('Ctrl Pts',(-12.3256628518317,58.9583333333333,-46.));
#15230=CARTESIAN_POINT('Ctrl Pts',(-2.81668763803891E-15,58.75,-46.));
#15231=CARTESIAN_POINT('Ctrl Pts',(12.3256628518316,58.5416666666667,-46.));
#15232=CARTESIAN_POINT('Ctrl Pts',(23.,58.3333333333333,-39.8371685740842));
#15233=CARTESIAN_POINT('Ctrl Pts',(33.6743371481683,58.125,-33.6743371481684));
#15234=CARTESIAN_POINT('Ctrl Pts',(39.8371685740842,57.9166666666667,-23.));
#15235=CARTESIAN_POINT('Ctrl Pts',(46.,57.7083333333333,-12.3256628518317));
#15236=CARTESIAN_POINT('Ctrl Pts',(46.,57.5,-5.63337527607782E-15));
#15237=CARTESIAN_POINT('Ctrl Pts',(46.,57.2916666666667,12.3256628518316));
#15238=CARTESIAN_POINT('Ctrl Pts',(39.8371685740842,57.0833333333333,23.));
#15239=CARTESIAN_POINT('Ctrl Pts',(33.6743371481684,56.875,33.6743371481683));
#15240=CARTESIAN_POINT('Ctrl Pts',(23.,56.6666666666667,39.8371685740842));
#15241=CARTESIAN_POINT('Ctrl Pts',(12.3256628518317,56.4583333333333,46.));
#15242=CARTESIAN_POINT('Ctrl Pts',(8.45006291411674E-15,56.25,46.));
#15243=CARTESIAN_POINT('Ctrl Pts',(-12.3256628518316,56.0416666666667,46.));
#15244=CARTESIAN_POINT('Ctrl Pts',(-23.,55.8333333333333,39.8371685740842));
#15245=CARTESIAN_POINT('Ctrl Pts',(-33.6743371481683,55.625,33.6743371481684));
#15246=CARTESIAN_POINT('Ctrl Pts',(-39.8371685740842,55.4166666666667,23.));
#15247=CARTESIAN_POINT('Ctrl Pts',(-46.,55.2083333333333,12.3256628518317));
#15248=CARTESIAN_POINT('Ctrl Pts',(-46.,55.,0.));
#15249=CARTESIAN_POINT('Ctrl Pts',(-46.,54.7916666666667,-12.3256628518316));
#15250=CARTESIAN_POINT('Ctrl Pts',(-39.8371685740842,54.5833333333333,-23.));
#15251=CARTESIAN_POINT('Ctrl Pts',(-33.6743371481684,54.375,-33.6743371481684));
#15252=CARTESIAN_POINT('Ctrl Pts',(-23.,54.1666666666667,-39.8371685740842));
#15253=CARTESIAN_POINT('Ctrl Pts',(-12.3256628518317,53.9583333333333,-46.));
#15254=CARTESIAN_POINT('Ctrl Pts',(-2.81668763803891E-15,53.75,-46.));
#15255=CARTESIAN_POINT('Ctrl Pts',(12.3256628518316,53.5416666666667,-46.));
#15256=CARTESIAN_POINT('Ctrl Pts',(23.,53.3333333333333,-39.8371685740842));
#15257=CARTESIAN_POINT('Ctrl Pts',(33.6743371481683,53.125,-33.6743371481684));
#15258=CARTESIAN_POINT('Ctrl Pts',(39.8371685740842,52.9166666666667,-23.));
#15259=CARTESIAN_POINT('Ctrl Pts',(46.,52.7083333333333,-12.3256628518317));
#15260=CARTESIAN_POINT('Ctrl Pts',(46.,52.5,-5.63337527607782E-15));
#15261=CARTESIAN_POINT('Ctrl Pts',(46.,52.2916666666667,12.3256628518316));
#15262=CARTESIAN_POINT('Ctrl Pts',(39.8371685740842,52.0833333333333,23.));
#15263=CARTESIAN_POINT('Ctrl Pts',(33.6743371481684,51.875,33.6743371481683));
#15264=CARTESIAN_POINT('Ctrl Pts',(23.,51.6666666666667,39.8371685740842));
#15265=CARTESIAN_POINT('Ctrl Pts',(12.3256628518317,51.4583333333333,46.));
#15266=CARTESIAN_POINT('Ctrl Pts',(8.45006291411674E-15,51.25,46.));
#15267=CARTESIAN_POINT('Ctrl Pts',(-12.3256628518316,51.0416666666667,46.));
#15268=CARTESIAN_POINT('Ctrl Pts',(-23.,50.8333333333333,39.8371685740842));
#15269=CARTESIAN_POINT('Ctrl Pts',(-33.6743371481683,50.625,33.6743371481684));
#15270=CARTESIAN_POINT('Ctrl Pts',(-39.8371685740842,50.4166666666667,23.));
#15271=CARTESIAN_POINT('Ctrl Pts',(-46.,50.2083333333333,12.3256628518317));
#15272=CARTESIAN_POINT('Ctrl Pts',(-46.,50.,0.));
#15273=CARTESIAN_POINT('Ctrl Pts',(-46.,49.7916666666667,-12.3256628518316));
#15274=CARTESIAN_POINT('Ctrl Pts',(-39.8371685740842,49.5833333333333,-23.));
#15275=CARTESIAN_POINT('Ctrl Pts',(-33.6743371481684,49.375,-33.6743371481684));
#15276=CARTESIAN_POINT('Ctrl Pts',(-23.,49.1666666666667,-39.8371685740842));
#15277=CARTESIAN_POINT('Ctrl Pts',(-12.3256628518317,48.9583333333333,-46.));
#15278=CARTESIAN_POINT('Ctrl Pts',(-2.81668763803891E-15,48.75,-46.));
#15279=CARTESIAN_POINT('Ctrl Pts',(12.3256628518316,48.5416666666667,-46.));
#15280=CARTESIAN_POINT('Ctrl Pts',(23.,48.3333333333333,-39.8371685740842));
#15281=CARTESIAN_POINT('Ctrl Pts',(33.6743371481683,48.125,-33.6743371481684));
#15282=CARTESIAN_POINT('Ctrl Pts',(39.8371685740842,47.9166666666667,-23.));
#15283=CARTESIAN_POINT('Ctrl Pts',(46.,47.7083333333333,-12.3256628518317));
#15284=CARTESIAN_POINT('Ctrl Pts',(46.,47.5,-5.63337527607782E-15));
#15285=CARTESIAN_POINT('Ctrl Pts',(46.,47.2916666666667,12.3256628518316));
#15286=CARTESIAN_POINT('Ctrl Pts',(39.8371685740842,47.0833333333333,23.));
#15287=CARTESIAN_POINT('Ctrl Pts',(33.6743371481684,46.875,33.6743371481683));
#15288=CARTESIAN_POINT('Ctrl Pts',(23.,46.6666666666667,39.8371685740842));
#15289=CARTESIAN_POINT('Ctrl Pts',(12.3256628518317,46.4583333333333,46.));
#15290=CARTESIAN_POINT('Ctrl Pts',(8.45006291411674E-15,46.25,46.));
#15291=CARTESIAN_POINT('Ctrl Pts',(-12.3256628518316,46.0416666666667,46.));
#15292=CARTESIAN_POINT('Ctrl Pts',(-23.,45.8333333333333,39.8371685740842));
#15293=CARTESIAN_POINT('Ctrl Pts',(-33.6743371481683,45.625,33.6743371481684));
#15294=CARTESIAN_POINT('Ctrl Pts',(-39.8371685740842,45.4166666666667,23.));
#15295=CARTESIAN_POINT('Ctrl Pts',(-46.,45.2083333333333,12.3256628518317));
#15296=CARTESIAN_POINT('Ctrl Pts',(-46.,45.,0.));
#15297=CARTESIAN_POINT('Ctrl Pts',(-46.,44.7916666666667,-12.3256628518316));
#15298=CARTESIAN_POINT('Ctrl Pts',(-39.8371685740842,44.5833333333333,-23.));
#15299=CARTESIAN_POINT('Ctrl Pts',(-33.6743371481684,44.375,-33.6743371481684));
#15300=CARTESIAN_POINT('Ctrl Pts',(-23.,44.1666666666667,-39.8371685740842));
#15301=CARTESIAN_POINT('Ctrl Pts',(-12.3256628518317,43.9583333333333,-46.));
#15302=CARTESIAN_POINT('Ctrl Pts',(-2.81668763803891E-15,43.75,-46.));
#15303=CARTESIAN_POINT('Ctrl Pts',(12.3256628518316,43.5416666666667,-46.));
#15304=CARTESIAN_POINT('Ctrl Pts',(23.,43.3333333333333,-39.8371685740842));
#15305=CARTESIAN_POINT('Ctrl Pts',(33.6743371481683,43.125,-33.6743371481684));
#15306=CARTESIAN_POINT('Ctrl Pts',(39.8371685740842,42.9166666666667,-23.));
#15307=CARTESIAN_POINT('Ctrl Pts',(46.,42.7083333333333,-12.3256628518317));
#15308=CARTESIAN_POINT('Ctrl Pts',(46.,42.5,-5.63337527607782E-15));
#15309=CARTESIAN_POINT('Ctrl Pts',(46.,42.2916666666667,12.3256628518316));
#15310=CARTESIAN_POINT('Ctrl Pts',(39.8371685740842,42.0833333333333,23.));
#15311=CARTESIAN_POINT('Ctrl Pts',(33.6743371481684,41.875,33.6743371481683));
#15312=CARTESIAN_POINT('Ctrl Pts',(23.,41.6666666666667,39.8371685740842));
#15313=CARTESIAN_POINT('Ctrl Pts',(12.3256628518317,41.4583333333333,46.));
#15314=CARTESIAN_POINT('Ctrl Pts',(8.45006291411674E-15,41.25,46.));
#15315=CARTESIAN_POINT('Ctrl Pts',(-12.3256628518316,41.0416666666667,46.));
#15316=CARTESIAN_POINT('Ctrl Pts',(-23.,40.8333333333333,39.8371685740842));
#15317=CARTESIAN_POINT('Ctrl Pts',(-33.6743371481683,40.625,33.6743371481684));
#15318=CARTESIAN_POINT('Ctrl Pts',(-39.8371685740842,40.4166666666667,23.));
#15319=CARTESIAN_POINT('Ctrl Pts',(-46.,40.2083333333333,12.3256628518317));
#15320=CARTESIAN_POINT('Ctrl Pts',(-46.,40.,0.));
#15321=CARTESIAN_POINT('Ctrl Pts',(-46.,39.7916666666667,-12.3256628518316));
#15322=CARTESIAN_POINT('Ctrl Pts',(-39.8371685740842,39.5833333333333,-23.));
#15323=CARTESIAN_POINT('Ctrl Pts',(-33.6743371481684,39.375,-33.6743371481684));
#15324=CARTESIAN_POINT('Ctrl Pts',(-23.,39.1666666666667,-39.8371685740842));
#15325=CARTESIAN_POINT('Ctrl Pts',(-12.3256628518317,38.9583333333333,-46.));
#15326=CARTESIAN_POINT('Ctrl Pts',(-2.81668763803891E-15,38.75,-46.));
#15327=CARTESIAN_POINT('Ctrl Pts',(12.3256628518316,38.5416666666667,-46.));
#15328=CARTESIAN_POINT('Ctrl Pts',(23.,38.3333333333333,-39.8371685740842));
#15329=CARTESIAN_POINT('Ctrl Pts',(33.6743371481683,38.125,-33.6743371481684));
#15330=CARTESIAN_POINT('Ctrl Pts',(39.8371685740842,37.9166666666667,-23.));
#15331=CARTESIAN_POINT('Ctrl Pts',(46.,37.7083333333333,-12.3256628518317));
#15332=CARTESIAN_POINT('Ctrl Pts',(46.,37.5,-5.63337527607782E-15));
#15333=CARTESIAN_POINT('Ctrl Pts',(46.,37.2916666666667,12.3256628518316));
#15334=CARTESIAN_POINT('Ctrl Pts',(39.8371685740842,37.0833333333333,23.));
#15335=CARTESIAN_POINT('Ctrl Pts',(33.6743371481684,36.875,33.6743371481683));
#15336=CARTESIAN_POINT('Ctrl Pts',(23.,36.6666666666667,39.8371685740842));
#15337=CARTESIAN_POINT('Ctrl Pts',(12.3256628518317,36.4583333333333,46.));
#15338=CARTESIAN_POINT('Ctrl Pts',(8.45006291411674E-15,36.25,46.));
#15339=CARTESIAN_POINT('Ctrl Pts',(-12.3256628518316,36.0416666666667,46.));
#15340=CARTESIAN_POINT('Ctrl Pts',(-23.,35.8333333333333,39.8371685740842));
#15341=CARTESIAN_POINT('Ctrl Pts',(-33.6743371481683,35.625,33.6743371481684));
#15342=CARTESIAN_POINT('Ctrl Pts',(-39.8371685740842,35.4166666666667,23.));
#15343=CARTESIAN_POINT('Ctrl Pts',(-46.,35.2083333333333,12.3256628518317));
#15344=CARTESIAN_POINT('Ctrl Pts',(-46.,35.,0.));
#15345=CARTESIAN_POINT('Ctrl Pts',(-46.,34.7916666666667,-12.3256628518316));
#15346=CARTESIAN_POINT('Ctrl Pts',(-39.8371685740842,34.5833333333333,-23.));
#15347=CARTESIAN_POINT('Ctrl Pts',(-33.6743371481684,34.375,-33.6743371481684));
#15348=CARTESIAN_POINT('Ctrl Pts',(-23.,34.1666666666667,-39.8371685740842));
#15349=CARTESIAN_POINT('Ctrl Pts',(-12.3256628518317,33.9583333333333,-46.));
#15350=CARTESIAN_POINT('Ctrl Pts',(-2.81668763803891E-15,33.75,-46.));
#15351=CARTESIAN_POINT('Ctrl Pts',(12.3256628518316,33.5416666666667,-46.));
#15352=CARTESIAN_POINT('Ctrl Pts',(23.,33.3333333333333,-39.8371685740842));
#15353=CARTESIAN_POINT('Ctrl Pts',(33.6743371481683,33.125,-33.6743371481684));
#15354=CARTESIAN_POINT('Ctrl Pts',(39.8371685740842,32.9166666666667,-23.));
#15355=CARTESIAN_POINT('Ctrl Pts',(46.,32.7083333333333,-12.3256628518317));
#15356=CARTESIAN_POINT('Ctrl Pts',(46.,32.5,-5.63337527607782E-15));
#15357=CARTESIAN_POINT('Ctrl Pts',(46.,32.2916666666667,12.3256628518316));
#15358=CARTESIAN_POINT('Ctrl Pts',(39.8371685740842,32.0833333333333,23.));
#15359=CARTESIAN_POINT('Ctrl Pts',(33.6743371481684,31.875,33.6743371481683));
#15360=CARTESIAN_POINT('Ctrl Pts',(23.,31.6666666666667,39.8371685740842));
#15361=CARTESIAN_POINT('Ctrl Pts',(12.3256628518317,31.4583333333333,46.));
#15362=CARTESIAN_POINT('Ctrl Pts',(8.45006291411674E-15,31.25,46.));
#15363=CARTESIAN_POINT('Ctrl Pts',(-12.3256628518316,31.0416666666667,46.));
#15364=CARTESIAN_POINT('Ctrl Pts',(-23.,30.8333333333333,39.8371685740842));
#15365=CARTESIAN_POINT('Ctrl Pts',(-33.6743371481683,30.625,33.6743371481684));
#15366=CARTESIAN_POINT('Ctrl Pts',(-39.8371685740842,30.4166666666667,23.));
#15367=CARTESIAN_POINT('Ctrl Pts',(-46.,30.2083333333333,12.3256628518317));
#15368=CARTESIAN_POINT('Ctrl Pts',(-46.,30.,0.));
#15369=CARTESIAN_POINT('Origin',(4513.80899804858,-7910.15855089474,-4.33048597777576));
#15370=CARTESIAN_POINT('Ctrl Pts',(-4.32456003949879,43.8240181593938,-45.7962681936506));
#15371=CARTESIAN_POINT('Ctrl Pts',(-4.32456003949876,43.6905125468623,-46.0278818021281));
#15372=CARTESIAN_POINT('Ctrl Pts',(-4.32456003949882,43.4234964717135,-46.4911062234486));
#15373=CARTESIAN_POINT('Ctrl Pts',(-4.32456003949885,43.1564711191154,-46.954325296818));
#15374=CARTESIAN_POINT('Ctrl Pts',(-4.32456003949885,42.7677643029224,-47.6286149142205));
#15375=CARTESIAN_POINT('Ctrl Pts',(-4.32456003949873,42.5125642776457,-48.0712916022845));
#15376=CARTESIAN_POINT('Ctrl Pts',(-4.32456003949873,42.2573567866782,-48.5139639861634));
#15377=CARTESIAN_POINT('Ctrl Pts',(-48.706329375,58.437500006828,-1.8898197019151E-14));
#15378=CARTESIAN_POINT('Ctrl Pts',(-48.706329375,58.2291666734946,-13.0508216223155));
#15379=CARTESIAN_POINT('Ctrl Pts',(-42.1809185638422,58.0208333401613,-24.3531646875));
#15380=CARTESIAN_POINT('Ctrl Pts',(-35.6555077526845,57.812500006828,-35.6555077526845));
#15381=CARTESIAN_POINT('Ctrl Pts',(-24.3531646875,57.6041666734946,-42.1809185638422));
#15382=CARTESIAN_POINT('Ctrl Pts',(-13.0508216223155,57.3958333401613,-48.706329375));
#15383=CARTESIAN_POINT('Ctrl Pts',(1.59157945007855E-14,57.187500006828,
-48.706329375));
#15384=CARTESIAN_POINT('Ctrl Pts',(13.0508216223155,56.9791666734946,-48.706329375));
#15385=CARTESIAN_POINT('Ctrl Pts',(24.3531646875,56.7708333401613,-42.1809185638422));
#15386=CARTESIAN_POINT('Ctrl Pts',(35.6555077526845,56.562500006828,-35.6555077526845));
#15387=CARTESIAN_POINT('Ctrl Pts',(42.1809185638422,56.3541666734946,-24.3531646875));
#15388=CARTESIAN_POINT('Ctrl Pts',(48.706329375,56.1458333401613,-13.0508216223155));
#15389=CARTESIAN_POINT('Ctrl Pts',(48.706329375,55.937500006828,1.293339198242E-14));
#15390=CARTESIAN_POINT('Ctrl Pts',(48.706329375,55.7291666734946,13.0508216223155));
#15391=CARTESIAN_POINT('Ctrl Pts',(42.1809185638422,55.5208333401613,24.3531646875));
#15392=CARTESIAN_POINT('Ctrl Pts',(35.6555077526845,55.312500006828,35.6555077526845));
#15393=CARTESIAN_POINT('Ctrl Pts',(24.3531646875,55.1041666734946,42.1809185638422));
#15394=CARTESIAN_POINT('Ctrl Pts',(13.0508216223155,54.8958333401613,48.706329375));
#15395=CARTESIAN_POINT('Ctrl Pts',(-9.95098946405443E-15,54.687500006828,
48.706329375));
#15396=CARTESIAN_POINT('Ctrl Pts',(-13.0508216223155,54.4791666734946,48.706329375));
#15397=CARTESIAN_POINT('Ctrl Pts',(-24.3531646875,54.2708333401613,42.1809185638423));
#15398=CARTESIAN_POINT('Ctrl Pts',(-35.6555077526845,54.062500006828,35.6555077526845));
#15399=CARTESIAN_POINT('Ctrl Pts',(-42.1809185638422,53.8541666734946,24.3531646875));
#15400=CARTESIAN_POINT('Ctrl Pts',(-48.706329375,53.6458333401613,13.0508216223155));
#15401=CARTESIAN_POINT('Ctrl Pts',(-48.706329375,53.437500006828,-1.8898197019151E-14));
#15402=CARTESIAN_POINT('Ctrl Pts',(-48.706329375,53.2291666734946,-13.0508216223155));
#15403=CARTESIAN_POINT('Ctrl Pts',(-42.1809185638422,53.0208333401613,-24.3531646875));
#15404=CARTESIAN_POINT('Ctrl Pts',(-35.6555077526845,52.812500006828,-35.6555077526845));
#15405=CARTESIAN_POINT('Ctrl Pts',(-24.3531646875,52.6041666734946,-42.1809185638422));
#15406=CARTESIAN_POINT('Ctrl Pts',(-13.0508216223155,52.3958333401613,-48.706329375));
#15407=CARTESIAN_POINT('Ctrl Pts',(1.59157945007855E-14,52.187500006828,
-48.706329375));
#15408=CARTESIAN_POINT('Ctrl Pts',(13.0508216223155,51.9791666734946,-48.706329375));
#15409=CARTESIAN_POINT('Ctrl Pts',(24.3531646875,51.7708333401613,-42.1809185638422));
#15410=CARTESIAN_POINT('Ctrl Pts',(35.6555077526845,51.562500006828,-35.6555077526845));
#15411=CARTESIAN_POINT('Ctrl Pts',(42.1809185638422,51.3541666734946,-24.3531646875));
#15412=CARTESIAN_POINT('Ctrl Pts',(48.706329375,51.1458333401613,-13.0508216223155));
#15413=CARTESIAN_POINT('Ctrl Pts',(48.706329375,50.937500006828,1.293339198242E-14));
#15414=CARTESIAN_POINT('Ctrl Pts',(48.706329375,50.7291666734946,13.0508216223155));
#15415=CARTESIAN_POINT('Ctrl Pts',(42.1809185638422,50.5208333401613,24.3531646875));
#15416=CARTESIAN_POINT('Ctrl Pts',(35.6555077526845,50.312500006828,35.6555077526845));
#15417=CARTESIAN_POINT('Ctrl Pts',(24.3531646875,50.1041666734946,42.1809185638422));
#15418=CARTESIAN_POINT('Ctrl Pts',(13.0508216223155,49.8958333401613,48.706329375));
#15419=CARTESIAN_POINT('Ctrl Pts',(-9.95098946405443E-15,49.687500006828,
48.706329375));
#15420=CARTESIAN_POINT('Ctrl Pts',(-13.0508216223155,49.4791666734946,48.706329375));
#15421=CARTESIAN_POINT('Ctrl Pts',(-24.3531646875,49.2708333401613,42.1809185638423));
#15422=CARTESIAN_POINT('Ctrl Pts',(-35.6555077526845,49.062500006828,35.6555077526845));
#15423=CARTESIAN_POINT('Ctrl Pts',(-42.1809185638422,48.8541666734946,24.3531646875));
#15424=CARTESIAN_POINT('Ctrl Pts',(-48.706329375,48.6458333401613,13.0508216223155));
#15425=CARTESIAN_POINT('Ctrl Pts',(-48.706329375,48.437500006828,-1.8898197019151E-14));
#15426=CARTESIAN_POINT('Ctrl Pts',(-48.706329375,48.2291666734946,-13.0508216223155));
#15427=CARTESIAN_POINT('Ctrl Pts',(-42.1809185638422,48.0208333401613,-24.3531646875));
#15428=CARTESIAN_POINT('Ctrl Pts',(-35.6555077526845,47.812500006828,-35.6555077526845));
#15429=CARTESIAN_POINT('Ctrl Pts',(-24.3531646875,47.6041666734946,-42.1809185638422));
#15430=CARTESIAN_POINT('Ctrl Pts',(-13.0508216223155,47.3958333401613,-48.706329375));
#15431=CARTESIAN_POINT('Ctrl Pts',(1.59157945007855E-14,47.187500006828,
-48.706329375));
#15432=CARTESIAN_POINT('Ctrl Pts',(13.0508216223155,46.9791666734946,-48.706329375));
#15433=CARTESIAN_POINT('Ctrl Pts',(24.3531646875,46.7708333401613,-42.1809185638422));
#15434=CARTESIAN_POINT('Ctrl Pts',(35.6555077526845,46.562500006828,-35.6555077526845));
#15435=CARTESIAN_POINT('Ctrl Pts',(42.1809185638422,46.3541666734946,-24.3531646875));
#15436=CARTESIAN_POINT('Ctrl Pts',(48.706329375,46.1458333401613,-13.0508216223155));
#15437=CARTESIAN_POINT('Ctrl Pts',(48.706329375,45.937500006828,1.293339198242E-14));
#15438=CARTESIAN_POINT('Ctrl Pts',(48.706329375,45.7291666734946,13.0508216223155));
#15439=CARTESIAN_POINT('Ctrl Pts',(42.1809185638422,45.5208333401613,24.3531646875));
#15440=CARTESIAN_POINT('Ctrl Pts',(35.6555077526845,45.312500006828,35.6555077526845));
#15441=CARTESIAN_POINT('Ctrl Pts',(24.3531646875,45.1041666734946,42.1809185638422));
#15442=CARTESIAN_POINT('Ctrl Pts',(13.0508216223155,44.8958333401613,48.706329375));
#15443=CARTESIAN_POINT('Ctrl Pts',(-9.95098946405443E-15,44.687500006828,
48.706329375));
#15444=CARTESIAN_POINT('Ctrl Pts',(-13.0508216223155,44.4791666734946,48.706329375));
#15445=CARTESIAN_POINT('Ctrl Pts',(-24.3531646875,44.2708333401613,42.1809185638423));
#15446=CARTESIAN_POINT('Ctrl Pts',(-35.6555077526845,44.062500006828,35.6555077526845));
#15447=CARTESIAN_POINT('Ctrl Pts',(-42.1809185638422,43.8541666734946,24.3531646875));
#15448=CARTESIAN_POINT('Ctrl Pts',(-48.706329375,43.6458333401613,13.0508216223155));
#15449=CARTESIAN_POINT('Ctrl Pts',(-48.706329375,43.437500006828,-1.8898197019151E-14));
#15450=CARTESIAN_POINT('Ctrl Pts',(-48.706329375,43.2291666734946,-13.0508216223155));
#15451=CARTESIAN_POINT('Ctrl Pts',(-42.1809185638422,43.0208333401613,-24.3531646875));
#15452=CARTESIAN_POINT('Ctrl Pts',(-35.6555077526845,42.812500006828,-35.6555077526845));
#15453=CARTESIAN_POINT('Ctrl Pts',(-24.3531646875,42.6041666734946,-42.1809185638422));
#15454=CARTESIAN_POINT('Ctrl Pts',(-13.0508216223155,42.3958333401613,-48.706329375));
#15455=CARTESIAN_POINT('Ctrl Pts',(1.59157945007855E-14,42.187500006828,
-48.706329375));
#15456=CARTESIAN_POINT('Ctrl Pts',(13.0508216223155,41.9791666734946,-48.706329375));
#15457=CARTESIAN_POINT('Ctrl Pts',(24.3531646875,41.7708333401613,-42.1809185638422));
#15458=CARTESIAN_POINT('Ctrl Pts',(35.6555077526845,41.562500006828,-35.6555077526845));
#15459=CARTESIAN_POINT('Ctrl Pts',(42.1809185638422,41.3541666734946,-24.3531646875));
#15460=CARTESIAN_POINT('Ctrl Pts',(48.706329375,41.1458333401613,-13.0508216223155));
#15461=CARTESIAN_POINT('Ctrl Pts',(48.706329375,40.937500006828,1.293339198242E-14));
#15462=CARTESIAN_POINT('Ctrl Pts',(48.706329375,40.7291666734946,13.0508216223155));
#15463=CARTESIAN_POINT('Ctrl Pts',(42.1809185638422,40.5208333401613,24.3531646875));
#15464=CARTESIAN_POINT('Ctrl Pts',(35.6555077526845,40.312500006828,35.6555077526845));
#15465=CARTESIAN_POINT('Ctrl Pts',(24.3531646875,40.1041666734946,42.1809185638422));
#15466=CARTESIAN_POINT('Ctrl Pts',(13.0508216223155,39.8958333401613,48.706329375));
#15467=CARTESIAN_POINT('Ctrl Pts',(-9.95098946405443E-15,39.687500006828,
48.706329375));
#15468=CARTESIAN_POINT('Ctrl Pts',(-13.0508216223155,39.4791666734946,48.706329375));
#15469=CARTESIAN_POINT('Ctrl Pts',(-24.3531646875,39.2708333401613,42.1809185638423));
#15470=CARTESIAN_POINT('Ctrl Pts',(-35.6555077526845,39.062500006828,35.6555077526845));
#15471=CARTESIAN_POINT('Ctrl Pts',(-42.1809185638422,38.8541666734946,24.3531646875));
#15472=CARTESIAN_POINT('Ctrl Pts',(-48.706329375,38.6458333401613,13.0508216223155));
#15473=CARTESIAN_POINT('Ctrl Pts',(-48.706329375,38.437500006828,-1.8898197019151E-14));
#15474=CARTESIAN_POINT('Ctrl Pts',(-48.706329375,38.2291666734946,-13.0508216223155));
#15475=CARTESIAN_POINT('Ctrl Pts',(-42.1809185638422,38.0208333401613,-24.3531646875));
#15476=CARTESIAN_POINT('Ctrl Pts',(-35.6555077526845,37.812500006828,-35.6555077526845));
#15477=CARTESIAN_POINT('Ctrl Pts',(-24.3531646875,37.6041666734946,-42.1809185638422));
#15478=CARTESIAN_POINT('Ctrl Pts',(-13.0508216223155,37.3958333401613,-48.706329375));
#15479=CARTESIAN_POINT('Ctrl Pts',(1.59157945007855E-14,37.187500006828,
-48.706329375));
#15480=CARTESIAN_POINT('Ctrl Pts',(13.0508216223155,36.9791666734946,-48.706329375));
#15481=CARTESIAN_POINT('Ctrl Pts',(24.3531646875,36.7708333401613,-42.1809185638422));
#15482=CARTESIAN_POINT('Ctrl Pts',(35.6555077526845,36.562500006828,-35.6555077526845));
#15483=CARTESIAN_POINT('Ctrl Pts',(42.1809185638422,36.3541666734946,-24.3531646875));
#15484=CARTESIAN_POINT('Ctrl Pts',(48.706329375,36.1458333401613,-13.0508216223155));
#15485=CARTESIAN_POINT('Ctrl Pts',(48.706329375,35.937500006828,1.293339198242E-14));
#15486=CARTESIAN_POINT('Ctrl Pts',(48.706329375,35.7291666734946,13.0508216223155));
#15487=CARTESIAN_POINT('Ctrl Pts',(42.1809185638422,35.5208333401613,24.3531646875));
#15488=CARTESIAN_POINT('Ctrl Pts',(35.6555077526845,35.312500006828,35.6555077526845));
#15489=CARTESIAN_POINT('Ctrl Pts',(24.3531646875,35.1041666734946,42.1809185638422));
#15490=CARTESIAN_POINT('Ctrl Pts',(13.0508216223155,34.8958333401613,48.706329375));
#15491=CARTESIAN_POINT('Ctrl Pts',(-9.95098946405443E-15,34.687500006828,
48.706329375));
#15492=CARTESIAN_POINT('Ctrl Pts',(-13.0508216223155,34.4791666734946,48.706329375));
#15493=CARTESIAN_POINT('Ctrl Pts',(-24.3531646875,34.2708333401613,42.1809185638423));
#15494=CARTESIAN_POINT('Ctrl Pts',(-35.6555077526845,34.062500006828,35.6555077526845));
#15495=CARTESIAN_POINT('Ctrl Pts',(-42.1809185638422,33.8541666734946,24.3531646875));
#15496=CARTESIAN_POINT('Ctrl Pts',(-48.706329375,33.6458333401613,13.0508216223155));
#15497=CARTESIAN_POINT('Ctrl Pts',(-48.706329375,33.437500006828,-1.8898197019151E-14));
#15498=CARTESIAN_POINT('Ctrl Pts',(-48.706329375,33.2291666734946,-13.0508216223155));
#15499=CARTESIAN_POINT('Ctrl Pts',(-42.1809185638422,33.0208333401613,-24.3531646875));
#15500=CARTESIAN_POINT('Ctrl Pts',(-35.6555077526845,32.812500006828,-35.6555077526845));
#15501=CARTESIAN_POINT('Ctrl Pts',(-24.3531646875,32.6041666734946,-42.1809185638422));
#15502=CARTESIAN_POINT('Ctrl Pts',(-13.0508216223155,32.3958333401613,-48.706329375));
#15503=CARTESIAN_POINT('Ctrl Pts',(1.59157945007855E-14,32.187500006828,
-48.706329375));
#15504=CARTESIAN_POINT('Ctrl Pts',(13.0508216223155,31.9791666734946,-48.706329375));
#15505=CARTESIAN_POINT('Ctrl Pts',(24.3531646875,31.7708333401613,-42.1809185638422));
#15506=CARTESIAN_POINT('Ctrl Pts',(35.6555077526845,31.562500006828,-35.6555077526845));
#15507=CARTESIAN_POINT('Ctrl Pts',(42.1809185638422,31.3541666734946,-24.3531646875));
#15508=CARTESIAN_POINT('Ctrl Pts',(48.706329375,31.1458333401613,-13.0508216223155));
#15509=CARTESIAN_POINT('Ctrl Pts',(48.706329375,30.937500006828,1.293339198242E-14));
#15510=CARTESIAN_POINT('Ctrl Pts',(48.706329375,30.7291666734946,13.0508216223155));
#15511=CARTESIAN_POINT('Ctrl Pts',(42.1809185638422,30.5208333401613,24.3531646875));
#15512=CARTESIAN_POINT('Ctrl Pts',(35.6555077526845,30.312500006828,35.6555077526845));
#15513=CARTESIAN_POINT('Ctrl Pts',(24.3531646875,30.1041666734946,42.1809185638422));
#15514=CARTESIAN_POINT('Ctrl Pts',(13.0508216223155,29.8958333401613,48.706329375));
#15515=CARTESIAN_POINT('Ctrl Pts',(-9.95098946405443E-15,29.687500006828,
48.706329375));
#15516=CARTESIAN_POINT('Ctrl Pts',(-13.0508216223155,29.4791666734946,48.706329375));
#15517=CARTESIAN_POINT('Ctrl Pts',(-24.3531646875,29.2708333401613,42.1809185638423));
#15518=CARTESIAN_POINT('Ctrl Pts',(-35.6555077526845,29.062500006828,35.6555077526845));
#15519=CARTESIAN_POINT('Ctrl Pts',(-42.1809185638422,28.8541666734946,24.3531646875));
#15520=CARTESIAN_POINT('Ctrl Pts',(-48.706329375,28.6458333401613,13.0508216223155));
#15521=CARTESIAN_POINT('Ctrl Pts',(-48.706329375,28.437500006828,-1.8898197019151E-14));
#15522=CARTESIAN_POINT('Ctrl Pts',(-46.,60.,0.));
#15523=CARTESIAN_POINT('Ctrl Pts',(-46.,59.7916666666667,-12.3256628518316));
#15524=CARTESIAN_POINT('Ctrl Pts',(-39.8371685740842,59.5833333333333,-23.));
#15525=CARTESIAN_POINT('Ctrl Pts',(-33.6743371481684,59.375,-33.6743371481684));
#15526=CARTESIAN_POINT('Ctrl Pts',(-23.,59.1666666666667,-39.8371685740842));
#15527=CARTESIAN_POINT('Ctrl Pts',(-12.3256628518317,58.9583333333333,-46.));
#15528=CARTESIAN_POINT('Ctrl Pts',(-2.81668763803891E-15,58.75,-46.));
#15529=CARTESIAN_POINT('Ctrl Pts',(12.3256628518316,58.5416666666667,-46.));
#15530=CARTESIAN_POINT('Ctrl Pts',(23.,58.3333333333333,-39.8371685740842));
#15531=CARTESIAN_POINT('Ctrl Pts',(33.6743371481683,58.125,-33.6743371481684));
#15532=CARTESIAN_POINT('Ctrl Pts',(39.8371685740842,57.9166666666667,-23.));
#15533=CARTESIAN_POINT('Ctrl Pts',(46.,57.7083333333333,-12.3256628518317));
#15534=CARTESIAN_POINT('Ctrl Pts',(46.,57.5,-5.63337527607782E-15));
#15535=CARTESIAN_POINT('Ctrl Pts',(46.,57.2916666666667,12.3256628518316));
#15536=CARTESIAN_POINT('Ctrl Pts',(39.8371685740842,57.0833333333333,23.));
#15537=CARTESIAN_POINT('Ctrl Pts',(33.6743371481684,56.875,33.6743371481683));
#15538=CARTESIAN_POINT('Ctrl Pts',(23.,56.6666666666667,39.8371685740842));
#15539=CARTESIAN_POINT('Ctrl Pts',(12.3256628518317,56.4583333333333,46.));
#15540=CARTESIAN_POINT('Ctrl Pts',(8.45006291411674E-15,56.25,46.));
#15541=CARTESIAN_POINT('Ctrl Pts',(-12.3256628518316,56.0416666666667,46.));
#15542=CARTESIAN_POINT('Ctrl Pts',(-23.,55.8333333333333,39.8371685740842));
#15543=CARTESIAN_POINT('Ctrl Pts',(-33.6743371481683,55.625,33.6743371481684));
#15544=CARTESIAN_POINT('Ctrl Pts',(-39.8371685740842,55.4166666666667,23.));
#15545=CARTESIAN_POINT('Ctrl Pts',(-46.,55.2083333333333,12.3256628518317));
#15546=CARTESIAN_POINT('Ctrl Pts',(-46.,55.,0.));
#15547=CARTESIAN_POINT('Ctrl Pts',(-46.,54.7916666666667,-12.3256628518316));
#15548=CARTESIAN_POINT('Ctrl Pts',(-39.8371685740842,54.5833333333333,-23.));
#15549=CARTESIAN_POINT('Ctrl Pts',(-33.6743371481684,54.375,-33.6743371481684));
#15550=CARTESIAN_POINT('Ctrl Pts',(-23.,54.1666666666667,-39.8371685740842));
#15551=CARTESIAN_POINT('Ctrl Pts',(-12.3256628518317,53.9583333333333,-46.));
#15552=CARTESIAN_POINT('Ctrl Pts',(-2.81668763803891E-15,53.75,-46.));
#15553=CARTESIAN_POINT('Ctrl Pts',(12.3256628518316,53.5416666666667,-46.));
#15554=CARTESIAN_POINT('Ctrl Pts',(23.,53.3333333333333,-39.8371685740842));
#15555=CARTESIAN_POINT('Ctrl Pts',(33.6743371481683,53.125,-33.6743371481684));
#15556=CARTESIAN_POINT('Ctrl Pts',(39.8371685740842,52.9166666666667,-23.));
#15557=CARTESIAN_POINT('Ctrl Pts',(46.,52.7083333333333,-12.3256628518317));
#15558=CARTESIAN_POINT('Ctrl Pts',(46.,52.5,-5.63337527607782E-15));
#15559=CARTESIAN_POINT('Ctrl Pts',(46.,52.2916666666667,12.3256628518316));
#15560=CARTESIAN_POINT('Ctrl Pts',(39.8371685740842,52.0833333333333,23.));
#15561=CARTESIAN_POINT('Ctrl Pts',(33.6743371481684,51.875,33.6743371481683));
#15562=CARTESIAN_POINT('Ctrl Pts',(23.,51.6666666666667,39.8371685740842));
#15563=CARTESIAN_POINT('Ctrl Pts',(12.3256628518317,51.4583333333333,46.));
#15564=CARTESIAN_POINT('Ctrl Pts',(8.45006291411674E-15,51.25,46.));
#15565=CARTESIAN_POINT('Ctrl Pts',(-12.3256628518316,51.0416666666667,46.));
#15566=CARTESIAN_POINT('Ctrl Pts',(-23.,50.8333333333333,39.8371685740842));
#15567=CARTESIAN_POINT('Ctrl Pts',(-33.6743371481683,50.625,33.6743371481684));
#15568=CARTESIAN_POINT('Ctrl Pts',(-39.8371685740842,50.4166666666667,23.));
#15569=CARTESIAN_POINT('Ctrl Pts',(-46.,50.2083333333333,12.3256628518317));
#15570=CARTESIAN_POINT('Ctrl Pts',(-46.,50.,0.));
#15571=CARTESIAN_POINT('Ctrl Pts',(-46.,49.7916666666667,-12.3256628518316));
#15572=CARTESIAN_POINT('Ctrl Pts',(-39.8371685740842,49.5833333333333,-23.));
#15573=CARTESIAN_POINT('Ctrl Pts',(-33.6743371481684,49.375,-33.6743371481684));
#15574=CARTESIAN_POINT('Ctrl Pts',(-23.,49.1666666666667,-39.8371685740842));
#15575=CARTESIAN_POINT('Ctrl Pts',(-12.3256628518317,48.9583333333333,-46.));
#15576=CARTESIAN_POINT('Ctrl Pts',(-2.81668763803891E-15,48.75,-46.));
#15577=CARTESIAN_POINT('Ctrl Pts',(12.3256628518316,48.5416666666667,-46.));
#15578=CARTESIAN_POINT('Ctrl Pts',(23.,48.3333333333333,-39.8371685740842));
#15579=CARTESIAN_POINT('Ctrl Pts',(33.6743371481683,48.125,-33.6743371481684));
#15580=CARTESIAN_POINT('Ctrl Pts',(39.8371685740842,47.9166666666667,-23.));
#15581=CARTESIAN_POINT('Ctrl Pts',(46.,47.7083333333333,-12.3256628518317));
#15582=CARTESIAN_POINT('Ctrl Pts',(46.,47.5,-5.63337527607782E-15));
#15583=CARTESIAN_POINT('Ctrl Pts',(46.,47.2916666666667,12.3256628518316));
#15584=CARTESIAN_POINT('Ctrl Pts',(39.8371685740842,47.0833333333333,23.));
#15585=CARTESIAN_POINT('Ctrl Pts',(33.6743371481684,46.875,33.6743371481683));
#15586=CARTESIAN_POINT('Ctrl Pts',(23.,46.6666666666667,39.8371685740842));
#15587=CARTESIAN_POINT('Ctrl Pts',(12.3256628518317,46.4583333333333,46.));
#15588=CARTESIAN_POINT('Ctrl Pts',(8.45006291411674E-15,46.25,46.));
#15589=CARTESIAN_POINT('Ctrl Pts',(-12.3256628518316,46.0416666666667,46.));
#15590=CARTESIAN_POINT('Ctrl Pts',(-23.,45.8333333333333,39.8371685740842));
#15591=CARTESIAN_POINT('Ctrl Pts',(-33.6743371481683,45.625,33.6743371481684));
#15592=CARTESIAN_POINT('Ctrl Pts',(-39.8371685740842,45.4166666666667,23.));
#15593=CARTESIAN_POINT('Ctrl Pts',(-46.,45.2083333333333,12.3256628518317));
#15594=CARTESIAN_POINT('Ctrl Pts',(-46.,45.,0.));
#15595=CARTESIAN_POINT('Ctrl Pts',(-46.,44.7916666666667,-12.3256628518316));
#15596=CARTESIAN_POINT('Ctrl Pts',(-39.8371685740842,44.5833333333333,-23.));
#15597=CARTESIAN_POINT('Ctrl Pts',(-33.6743371481684,44.375,-33.6743371481684));
#15598=CARTESIAN_POINT('Ctrl Pts',(-23.,44.1666666666667,-39.8371685740842));
#15599=CARTESIAN_POINT('Ctrl Pts',(-12.3256628518317,43.9583333333333,-46.));
#15600=CARTESIAN_POINT('Ctrl Pts',(-2.81668763803891E-15,43.75,-46.));
#15601=CARTESIAN_POINT('Ctrl Pts',(12.3256628518316,43.5416666666667,-46.));
#15602=CARTESIAN_POINT('Ctrl Pts',(23.,43.3333333333333,-39.8371685740842));
#15603=CARTESIAN_POINT('Ctrl Pts',(33.6743371481683,43.125,-33.6743371481684));
#15604=CARTESIAN_POINT('Ctrl Pts',(39.8371685740842,42.9166666666667,-23.));
#15605=CARTESIAN_POINT('Ctrl Pts',(46.,42.7083333333333,-12.3256628518317));
#15606=CARTESIAN_POINT('Ctrl Pts',(46.,42.5,-5.63337527607782E-15));
#15607=CARTESIAN_POINT('Ctrl Pts',(46.,42.2916666666667,12.3256628518316));
#15608=CARTESIAN_POINT('Ctrl Pts',(39.8371685740842,42.0833333333333,23.));
#15609=CARTESIAN_POINT('Ctrl Pts',(33.6743371481684,41.875,33.6743371481683));
#15610=CARTESIAN_POINT('Ctrl Pts',(23.,41.6666666666667,39.8371685740842));
#15611=CARTESIAN_POINT('Ctrl Pts',(12.3256628518317,41.4583333333333,46.));
#15612=CARTESIAN_POINT('Ctrl Pts',(8.45006291411674E-15,41.25,46.));
#15613=CARTESIAN_POINT('Ctrl Pts',(-12.3256628518316,41.0416666666667,46.));
#15614=CARTESIAN_POINT('Ctrl Pts',(-23.,40.8333333333333,39.8371685740842));
#15615=CARTESIAN_POINT('Ctrl Pts',(-33.6743371481683,40.625,33.6743371481684));
#15616=CARTESIAN_POINT('Ctrl Pts',(-39.8371685740842,40.4166666666667,23.));
#15617=CARTESIAN_POINT('Ctrl Pts',(-46.,40.2083333333333,12.3256628518317));
#15618=CARTESIAN_POINT('Ctrl Pts',(-46.,40.,0.));
#15619=CARTESIAN_POINT('Ctrl Pts',(-46.,39.7916666666667,-12.3256628518316));
#15620=CARTESIAN_POINT('Ctrl Pts',(-39.8371685740842,39.5833333333333,-23.));
#15621=CARTESIAN_POINT('Ctrl Pts',(-33.6743371481684,39.375,-33.6743371481684));
#15622=CARTESIAN_POINT('Ctrl Pts',(-23.,39.1666666666667,-39.8371685740842));
#15623=CARTESIAN_POINT('Ctrl Pts',(-12.3256628518317,38.9583333333333,-46.));
#15624=CARTESIAN_POINT('Ctrl Pts',(-2.81668763803891E-15,38.75,-46.));
#15625=CARTESIAN_POINT('Ctrl Pts',(12.3256628518316,38.5416666666667,-46.));
#15626=CARTESIAN_POINT('Ctrl Pts',(23.,38.3333333333333,-39.8371685740842));
#15627=CARTESIAN_POINT('Ctrl Pts',(33.6743371481683,38.125,-33.6743371481684));
#15628=CARTESIAN_POINT('Ctrl Pts',(39.8371685740842,37.9166666666667,-23.));
#15629=CARTESIAN_POINT('Ctrl Pts',(46.,37.7083333333333,-12.3256628518317));
#15630=CARTESIAN_POINT('Ctrl Pts',(46.,37.5,-5.63337527607782E-15));
#15631=CARTESIAN_POINT('Ctrl Pts',(46.,37.2916666666667,12.3256628518316));
#15632=CARTESIAN_POINT('Ctrl Pts',(39.8371685740842,37.0833333333333,23.));
#15633=CARTESIAN_POINT('Ctrl Pts',(33.6743371481684,36.875,33.6743371481683));
#15634=CARTESIAN_POINT('Ctrl Pts',(23.,36.6666666666667,39.8371685740842));
#15635=CARTESIAN_POINT('Ctrl Pts',(12.3256628518317,36.4583333333333,46.));
#15636=CARTESIAN_POINT('Ctrl Pts',(8.45006291411674E-15,36.25,46.));
#15637=CARTESIAN_POINT('Ctrl Pts',(-12.3256628518316,36.0416666666667,46.));
#15638=CARTESIAN_POINT('Ctrl Pts',(-23.,35.8333333333333,39.8371685740842));
#15639=CARTESIAN_POINT('Ctrl Pts',(-33.6743371481683,35.625,33.6743371481684));
#15640=CARTESIAN_POINT('Ctrl Pts',(-39.8371685740842,35.4166666666667,23.));
#15641=CARTESIAN_POINT('Ctrl Pts',(-46.,35.2083333333333,12.3256628518317));
#15642=CARTESIAN_POINT('Ctrl Pts',(-46.,35.,0.));
#15643=CARTESIAN_POINT('Ctrl Pts',(-46.,34.7916666666667,-12.3256628518316));
#15644=CARTESIAN_POINT('Ctrl Pts',(-39.8371685740842,34.5833333333333,-23.));
#15645=CARTESIAN_POINT('Ctrl Pts',(-33.6743371481684,34.375,-33.6743371481684));
#15646=CARTESIAN_POINT('Ctrl Pts',(-23.,34.1666666666667,-39.8371685740842));
#15647=CARTESIAN_POINT('Ctrl Pts',(-12.3256628518317,33.9583333333333,-46.));
#15648=CARTESIAN_POINT('Ctrl Pts',(-2.81668763803891E-15,33.75,-46.));
#15649=CARTESIAN_POINT('Ctrl Pts',(12.3256628518316,33.5416666666667,-46.));
#15650=CARTESIAN_POINT('Ctrl Pts',(23.,33.3333333333333,-39.8371685740842));
#15651=CARTESIAN_POINT('Ctrl Pts',(33.6743371481683,33.125,-33.6743371481684));
#15652=CARTESIAN_POINT('Ctrl Pts',(39.8371685740842,32.9166666666667,-23.));
#15653=CARTESIAN_POINT('Ctrl Pts',(46.,32.7083333333333,-12.3256628518317));
#15654=CARTESIAN_POINT('Ctrl Pts',(46.,32.5,-5.63337527607782E-15));
#15655=CARTESIAN_POINT('Ctrl Pts',(46.,32.2916666666667,12.3256628518316));
#15656=CARTESIAN_POINT('Ctrl Pts',(39.8371685740842,32.0833333333333,23.));
#15657=CARTESIAN_POINT('Ctrl Pts',(33.6743371481684,31.875,33.6743371481683));
#15658=CARTESIAN_POINT('Ctrl Pts',(23.,31.6666666666667,39.8371685740842));
#15659=CARTESIAN_POINT('Ctrl Pts',(12.3256628518317,31.4583333333333,46.));
#15660=CARTESIAN_POINT('Ctrl Pts',(8.45006291411674E-15,31.25,46.));
#15661=CARTESIAN_POINT('Ctrl Pts',(-12.3256628518316,31.0416666666667,46.));
#15662=CARTESIAN_POINT('Ctrl Pts',(-23.,30.8333333333333,39.8371685740842));
#15663=CARTESIAN_POINT('Ctrl Pts',(-33.6743371481683,30.625,33.6743371481684));
#15664=CARTESIAN_POINT('Ctrl Pts',(-39.8371685740842,30.4166666666667,23.));
#15665=CARTESIAN_POINT('Ctrl Pts',(-46.,30.2083333333333,12.3256628518317));
#15666=CARTESIAN_POINT('Ctrl Pts',(-46.,30.,0.));
#15667=CARTESIAN_POINT('Ctrl Pts',(-45.858362923034,45.061608680256,3.60701400320326));
#15668=CARTESIAN_POINT('Ctrl Pts',(-46.089925771934,44.9280150456296,3.60701400320326));
#15669=CARTESIAN_POINT('Ctrl Pts',(-46.5530501979845,44.6608255719955,3.60701400320326));
#15670=CARTESIAN_POINT('Ctrl Pts',(-47.0161721905706,44.3936318804496,3.60701400320324));
#15671=CARTESIAN_POINT('Ctrl Pts',(-47.6893519862319,44.0052434879083,3.60701400320324));
#15672=CARTESIAN_POINT('Ctrl Pts',(-48.1309692507095,43.7504492807381,3.60701400320326));
#15673=CARTESIAN_POINT('Ctrl Pts',(-48.5725845633798,43.4956516907297,3.60701400320326));
#15674=CARTESIAN_POINT('Origin',(-4.32455996307467,-7926.57953929723,-4524.0108731871));
#15675=CARTESIAN_POINT('Ctrl Pts',(-48.706329375,58.437500006828,-1.8898197019151E-14));
#15676=CARTESIAN_POINT('Ctrl Pts',(-48.706329375,58.2291666734946,-13.0508216223155));
#15677=CARTESIAN_POINT('Ctrl Pts',(-42.1809185638422,58.0208333401613,-24.3531646875));
#15678=CARTESIAN_POINT('Ctrl Pts',(-35.6555077526845,57.812500006828,-35.6555077526845));
#15679=CARTESIAN_POINT('Ctrl Pts',(-24.3531646875,57.6041666734946,-42.1809185638422));
#15680=CARTESIAN_POINT('Ctrl Pts',(-13.0508216223155,57.3958333401613,-48.706329375));
#15681=CARTESIAN_POINT('Ctrl Pts',(1.59157945007855E-14,57.187500006828,
-48.706329375));
#15682=CARTESIAN_POINT('Ctrl Pts',(13.0508216223155,56.9791666734946,-48.706329375));
#15683=CARTESIAN_POINT('Ctrl Pts',(24.3531646875,56.7708333401613,-42.1809185638422));
#15684=CARTESIAN_POINT('Ctrl Pts',(35.6555077526845,56.562500006828,-35.6555077526845));
#15685=CARTESIAN_POINT('Ctrl Pts',(42.1809185638422,56.3541666734946,-24.3531646875));
#15686=CARTESIAN_POINT('Ctrl Pts',(48.706329375,56.1458333401613,-13.0508216223155));
#15687=CARTESIAN_POINT('Ctrl Pts',(48.706329375,55.937500006828,1.293339198242E-14));
#15688=CARTESIAN_POINT('Ctrl Pts',(48.706329375,55.7291666734946,13.0508216223155));
#15689=CARTESIAN_POINT('Ctrl Pts',(42.1809185638422,55.5208333401613,24.3531646875));
#15690=CARTESIAN_POINT('Ctrl Pts',(35.6555077526845,55.312500006828,35.6555077526845));
#15691=CARTESIAN_POINT('Ctrl Pts',(24.3531646875,55.1041666734946,42.1809185638422));
#15692=CARTESIAN_POINT('Ctrl Pts',(13.0508216223155,54.8958333401613,48.706329375));
#15693=CARTESIAN_POINT('Ctrl Pts',(-9.95098946405443E-15,54.687500006828,
48.706329375));
#15694=CARTESIAN_POINT('Ctrl Pts',(-13.0508216223155,54.4791666734946,48.706329375));
#15695=CARTESIAN_POINT('Ctrl Pts',(-24.3531646875,54.2708333401613,42.1809185638423));
#15696=CARTESIAN_POINT('Ctrl Pts',(-35.6555077526845,54.062500006828,35.6555077526845));
#15697=CARTESIAN_POINT('Ctrl Pts',(-42.1809185638422,53.8541666734946,24.3531646875));
#15698=CARTESIAN_POINT('Ctrl Pts',(-48.706329375,53.6458333401613,13.0508216223155));
#15699=CARTESIAN_POINT('Ctrl Pts',(-48.706329375,53.437500006828,-1.8898197019151E-14));
#15700=CARTESIAN_POINT('Ctrl Pts',(-48.706329375,53.2291666734946,-13.0508216223155));
#15701=CARTESIAN_POINT('Ctrl Pts',(-42.1809185638422,53.0208333401613,-24.3531646875));
#15702=CARTESIAN_POINT('Ctrl Pts',(-35.6555077526845,52.812500006828,-35.6555077526845));
#15703=CARTESIAN_POINT('Ctrl Pts',(-24.3531646875,52.6041666734946,-42.1809185638422));
#15704=CARTESIAN_POINT('Ctrl Pts',(-13.0508216223155,52.3958333401613,-48.706329375));
#15705=CARTESIAN_POINT('Ctrl Pts',(1.59157945007855E-14,52.187500006828,
-48.706329375));
#15706=CARTESIAN_POINT('Ctrl Pts',(13.0508216223155,51.9791666734946,-48.706329375));
#15707=CARTESIAN_POINT('Ctrl Pts',(24.3531646875,51.7708333401613,-42.1809185638422));
#15708=CARTESIAN_POINT('Ctrl Pts',(35.6555077526845,51.562500006828,-35.6555077526845));
#15709=CARTESIAN_POINT('Ctrl Pts',(42.1809185638422,51.3541666734946,-24.3531646875));
#15710=CARTESIAN_POINT('Ctrl Pts',(48.706329375,51.1458333401613,-13.0508216223155));
#15711=CARTESIAN_POINT('Ctrl Pts',(48.706329375,50.937500006828,1.293339198242E-14));
#15712=CARTESIAN_POINT('Ctrl Pts',(48.706329375,50.7291666734946,13.0508216223155));
#15713=CARTESIAN_POINT('Ctrl Pts',(42.1809185638422,50.5208333401613,24.3531646875));
#15714=CARTESIAN_POINT('Ctrl Pts',(35.6555077526845,50.312500006828,35.6555077526845));
#15715=CARTESIAN_POINT('Ctrl Pts',(24.3531646875,50.1041666734946,42.1809185638422));
#15716=CARTESIAN_POINT('Ctrl Pts',(13.0508216223155,49.8958333401613,48.706329375));
#15717=CARTESIAN_POINT('Ctrl Pts',(-9.95098946405443E-15,49.687500006828,
48.706329375));
#15718=CARTESIAN_POINT('Ctrl Pts',(-13.0508216223155,49.4791666734946,48.706329375));
#15719=CARTESIAN_POINT('Ctrl Pts',(-24.3531646875,49.2708333401613,42.1809185638423));
#15720=CARTESIAN_POINT('Ctrl Pts',(-35.6555077526845,49.062500006828,35.6555077526845));
#15721=CARTESIAN_POINT('Ctrl Pts',(-42.1809185638422,48.8541666734946,24.3531646875));
#15722=CARTESIAN_POINT('Ctrl Pts',(-48.706329375,48.6458333401613,13.0508216223155));
#15723=CARTESIAN_POINT('Ctrl Pts',(-48.706329375,48.437500006828,-1.8898197019151E-14));
#15724=CARTESIAN_POINT('Ctrl Pts',(-48.706329375,48.2291666734946,-13.0508216223155));
#15725=CARTESIAN_POINT('Ctrl Pts',(-42.1809185638422,48.0208333401613,-24.3531646875));
#15726=CARTESIAN_POINT('Ctrl Pts',(-35.6555077526845,47.812500006828,-35.6555077526845));
#15727=CARTESIAN_POINT('Ctrl Pts',(-24.3531646875,47.6041666734946,-42.1809185638422));
#15728=CARTESIAN_POINT('Ctrl Pts',(-13.0508216223155,47.3958333401613,-48.706329375));
#15729=CARTESIAN_POINT('Ctrl Pts',(1.59157945007855E-14,47.187500006828,
-48.706329375));
#15730=CARTESIAN_POINT('Ctrl Pts',(13.0508216223155,46.9791666734946,-48.706329375));
#15731=CARTESIAN_POINT('Ctrl Pts',(24.3531646875,46.7708333401613,-42.1809185638422));
#15732=CARTESIAN_POINT('Ctrl Pts',(35.6555077526845,46.562500006828,-35.6555077526845));
#15733=CARTESIAN_POINT('Ctrl Pts',(42.1809185638422,46.3541666734946,-24.3531646875));
#15734=CARTESIAN_POINT('Ctrl Pts',(48.706329375,46.1458333401613,-13.0508216223155));
#15735=CARTESIAN_POINT('Ctrl Pts',(48.706329375,45.937500006828,1.293339198242E-14));
#15736=CARTESIAN_POINT('Ctrl Pts',(48.706329375,45.7291666734946,13.0508216223155));
#15737=CARTESIAN_POINT('Ctrl Pts',(42.1809185638422,45.5208333401613,24.3531646875));
#15738=CARTESIAN_POINT('Ctrl Pts',(35.6555077526845,45.312500006828,35.6555077526845));
#15739=CARTESIAN_POINT('Ctrl Pts',(24.3531646875,45.1041666734946,42.1809185638422));
#15740=CARTESIAN_POINT('Ctrl Pts',(13.0508216223155,44.8958333401613,48.706329375));
#15741=CARTESIAN_POINT('Ctrl Pts',(-9.95098946405443E-15,44.687500006828,
48.706329375));
#15742=CARTESIAN_POINT('Ctrl Pts',(-13.0508216223155,44.4791666734946,48.706329375));
#15743=CARTESIAN_POINT('Ctrl Pts',(-24.3531646875,44.2708333401613,42.1809185638423));
#15744=CARTESIAN_POINT('Ctrl Pts',(-35.6555077526845,44.062500006828,35.6555077526845));
#15745=CARTESIAN_POINT('Ctrl Pts',(-42.1809185638422,43.8541666734946,24.3531646875));
#15746=CARTESIAN_POINT('Ctrl Pts',(-48.706329375,43.6458333401613,13.0508216223155));
#15747=CARTESIAN_POINT('Ctrl Pts',(-48.706329375,43.437500006828,-1.8898197019151E-14));
#15748=CARTESIAN_POINT('Ctrl Pts',(-48.706329375,43.2291666734946,-13.0508216223155));
#15749=CARTESIAN_POINT('Ctrl Pts',(-42.1809185638422,43.0208333401613,-24.3531646875));
#15750=CARTESIAN_POINT('Ctrl Pts',(-35.6555077526845,42.812500006828,-35.6555077526845));
#15751=CARTESIAN_POINT('Ctrl Pts',(-24.3531646875,42.6041666734946,-42.1809185638422));
#15752=CARTESIAN_POINT('Ctrl Pts',(-13.0508216223155,42.3958333401613,-48.706329375));
#15753=CARTESIAN_POINT('Ctrl Pts',(1.59157945007855E-14,42.187500006828,
-48.706329375));
#15754=CARTESIAN_POINT('Ctrl Pts',(13.0508216223155,41.9791666734946,-48.706329375));
#15755=CARTESIAN_POINT('Ctrl Pts',(24.3531646875,41.7708333401613,-42.1809185638422));
#15756=CARTESIAN_POINT('Ctrl Pts',(35.6555077526845,41.562500006828,-35.6555077526845));
#15757=CARTESIAN_POINT('Ctrl Pts',(42.1809185638422,41.3541666734946,-24.3531646875));
#15758=CARTESIAN_POINT('Ctrl Pts',(48.706329375,41.1458333401613,-13.0508216223155));
#15759=CARTESIAN_POINT('Ctrl Pts',(48.706329375,40.937500006828,1.293339198242E-14));
#15760=CARTESIAN_POINT('Ctrl Pts',(48.706329375,40.7291666734946,13.0508216223155));
#15761=CARTESIAN_POINT('Ctrl Pts',(42.1809185638422,40.5208333401613,24.3531646875));
#15762=CARTESIAN_POINT('Ctrl Pts',(35.6555077526845,40.312500006828,35.6555077526845));
#15763=CARTESIAN_POINT('Ctrl Pts',(24.3531646875,40.1041666734946,42.1809185638422));
#15764=CARTESIAN_POINT('Ctrl Pts',(13.0508216223155,39.8958333401613,48.706329375));
#15765=CARTESIAN_POINT('Ctrl Pts',(-9.95098946405443E-15,39.687500006828,
48.706329375));
#15766=CARTESIAN_POINT('Ctrl Pts',(-13.0508216223155,39.4791666734946,48.706329375));
#15767=CARTESIAN_POINT('Ctrl Pts',(-24.3531646875,39.2708333401613,42.1809185638423));
#15768=CARTESIAN_POINT('Ctrl Pts',(-35.6555077526845,39.062500006828,35.6555077526845));
#15769=CARTESIAN_POINT('Ctrl Pts',(-42.1809185638422,38.8541666734946,24.3531646875));
#15770=CARTESIAN_POINT('Ctrl Pts',(-48.706329375,38.6458333401613,13.0508216223155));
#15771=CARTESIAN_POINT('Ctrl Pts',(-48.706329375,38.437500006828,-1.8898197019151E-14));
#15772=CARTESIAN_POINT('Ctrl Pts',(-48.706329375,38.2291666734946,-13.0508216223155));
#15773=CARTESIAN_POINT('Ctrl Pts',(-42.1809185638422,38.0208333401613,-24.3531646875));
#15774=CARTESIAN_POINT('Ctrl Pts',(-35.6555077526845,37.812500006828,-35.6555077526845));
#15775=CARTESIAN_POINT('Ctrl Pts',(-24.3531646875,37.6041666734946,-42.1809185638422));
#15776=CARTESIAN_POINT('Ctrl Pts',(-13.0508216223155,37.3958333401613,-48.706329375));
#15777=CARTESIAN_POINT('Ctrl Pts',(1.59157945007855E-14,37.187500006828,
-48.706329375));
#15778=CARTESIAN_POINT('Ctrl Pts',(13.0508216223155,36.9791666734946,-48.706329375));
#15779=CARTESIAN_POINT('Ctrl Pts',(24.3531646875,36.7708333401613,-42.1809185638422));
#15780=CARTESIAN_POINT('Ctrl Pts',(35.6555077526845,36.562500006828,-35.6555077526845));
#15781=CARTESIAN_POINT('Ctrl Pts',(42.1809185638422,36.3541666734946,-24.3531646875));
#15782=CARTESIAN_POINT('Ctrl Pts',(48.706329375,36.1458333401613,-13.0508216223155));
#15783=CARTESIAN_POINT('Ctrl Pts',(48.706329375,35.937500006828,1.293339198242E-14));
#15784=CARTESIAN_POINT('Ctrl Pts',(48.706329375,35.7291666734946,13.0508216223155));
#15785=CARTESIAN_POINT('Ctrl Pts',(42.1809185638422,35.5208333401613,24.3531646875));
#15786=CARTESIAN_POINT('Ctrl Pts',(35.6555077526845,35.312500006828,35.6555077526845));
#15787=CARTESIAN_POINT('Ctrl Pts',(24.3531646875,35.1041666734946,42.1809185638422));
#15788=CARTESIAN_POINT('Ctrl Pts',(13.0508216223155,34.8958333401613,48.706329375));
#15789=CARTESIAN_POINT('Ctrl Pts',(-9.95098946405443E-15,34.687500006828,
48.706329375));
#15790=CARTESIAN_POINT('Ctrl Pts',(-13.0508216223155,34.4791666734946,48.706329375));
#15791=CARTESIAN_POINT('Ctrl Pts',(-24.3531646875,34.2708333401613,42.1809185638423));
#15792=CARTESIAN_POINT('Ctrl Pts',(-35.6555077526845,34.062500006828,35.6555077526845));
#15793=CARTESIAN_POINT('Ctrl Pts',(-42.1809185638422,33.8541666734946,24.3531646875));
#15794=CARTESIAN_POINT('Ctrl Pts',(-48.706329375,33.6458333401613,13.0508216223155));
#15795=CARTESIAN_POINT('Ctrl Pts',(-48.706329375,33.437500006828,-1.8898197019151E-14));
#15796=CARTESIAN_POINT('Ctrl Pts',(-48.706329375,33.2291666734946,-13.0508216223155));
#15797=CARTESIAN_POINT('Ctrl Pts',(-42.1809185638422,33.0208333401613,-24.3531646875));
#15798=CARTESIAN_POINT('Ctrl Pts',(-35.6555077526845,32.812500006828,-35.6555077526845));
#15799=CARTESIAN_POINT('Ctrl Pts',(-24.3531646875,32.6041666734946,-42.1809185638422));
#15800=CARTESIAN_POINT('Ctrl Pts',(-13.0508216223155,32.3958333401613,-48.706329375));
#15801=CARTESIAN_POINT('Ctrl Pts',(1.59157945007855E-14,32.187500006828,
-48.706329375));
#15802=CARTESIAN_POINT('Ctrl Pts',(13.0508216223155,31.9791666734946,-48.706329375));
#15803=CARTESIAN_POINT('Ctrl Pts',(24.3531646875,31.7708333401613,-42.1809185638422));
#15804=CARTESIAN_POINT('Ctrl Pts',(35.6555077526845,31.562500006828,-35.6555077526845));
#15805=CARTESIAN_POINT('Ctrl Pts',(42.1809185638422,31.3541666734946,-24.3531646875));
#15806=CARTESIAN_POINT('Ctrl Pts',(48.706329375,31.1458333401613,-13.0508216223155));
#15807=CARTESIAN_POINT('Ctrl Pts',(48.706329375,30.937500006828,1.293339198242E-14));
#15808=CARTESIAN_POINT('Ctrl Pts',(48.706329375,30.7291666734946,13.0508216223155));
#15809=CARTESIAN_POINT('Ctrl Pts',(42.1809185638422,30.5208333401613,24.3531646875));
#15810=CARTESIAN_POINT('Ctrl Pts',(35.6555077526845,30.312500006828,35.6555077526845));
#15811=CARTESIAN_POINT('Ctrl Pts',(24.3531646875,30.1041666734946,42.1809185638422));
#15812=CARTESIAN_POINT('Ctrl Pts',(13.0508216223155,29.8958333401613,48.706329375));
#15813=CARTESIAN_POINT('Ctrl Pts',(-9.95098946405443E-15,29.687500006828,
48.706329375));
#15814=CARTESIAN_POINT('Ctrl Pts',(-13.0508216223155,29.4791666734946,48.706329375));
#15815=CARTESIAN_POINT('Ctrl Pts',(-24.3531646875,29.2708333401613,42.1809185638423));
#15816=CARTESIAN_POINT('Ctrl Pts',(-35.6555077526845,29.062500006828,35.6555077526845));
#15817=CARTESIAN_POINT('Ctrl Pts',(-42.1809185638422,28.8541666734946,24.3531646875));
#15818=CARTESIAN_POINT('Ctrl Pts',(-48.706329375,28.6458333401613,13.0508216223155));
#15819=CARTESIAN_POINT('Ctrl Pts',(-48.706329375,28.437500006828,-1.8898197019151E-14));
#15820=CARTESIAN_POINT('Ctrl Pts',(-46.,60.,0.));
#15821=CARTESIAN_POINT('Ctrl Pts',(-46.,59.7916666666667,-12.3256628518316));
#15822=CARTESIAN_POINT('Ctrl Pts',(-39.8371685740842,59.5833333333333,-23.));
#15823=CARTESIAN_POINT('Ctrl Pts',(-33.6743371481684,59.375,-33.6743371481684));
#15824=CARTESIAN_POINT('Ctrl Pts',(-23.,59.1666666666667,-39.8371685740842));
#15825=CARTESIAN_POINT('Ctrl Pts',(-12.3256628518317,58.9583333333333,-46.));
#15826=CARTESIAN_POINT('Ctrl Pts',(-2.81668763803891E-15,58.75,-46.));
#15827=CARTESIAN_POINT('Ctrl Pts',(12.3256628518316,58.5416666666667,-46.));
#15828=CARTESIAN_POINT('Ctrl Pts',(23.,58.3333333333333,-39.8371685740842));
#15829=CARTESIAN_POINT('Ctrl Pts',(33.6743371481683,58.125,-33.6743371481684));
#15830=CARTESIAN_POINT('Ctrl Pts',(39.8371685740842,57.9166666666667,-23.));
#15831=CARTESIAN_POINT('Ctrl Pts',(46.,57.7083333333333,-12.3256628518317));
#15832=CARTESIAN_POINT('Ctrl Pts',(46.,57.5,-5.63337527607782E-15));
#15833=CARTESIAN_POINT('Ctrl Pts',(46.,57.2916666666667,12.3256628518316));
#15834=CARTESIAN_POINT('Ctrl Pts',(39.8371685740842,57.0833333333333,23.));
#15835=CARTESIAN_POINT('Ctrl Pts',(33.6743371481684,56.875,33.6743371481683));
#15836=CARTESIAN_POINT('Ctrl Pts',(23.,56.6666666666667,39.8371685740842));
#15837=CARTESIAN_POINT('Ctrl Pts',(12.3256628518317,56.4583333333333,46.));
#15838=CARTESIAN_POINT('Ctrl Pts',(8.45006291411674E-15,56.25,46.));
#15839=CARTESIAN_POINT('Ctrl Pts',(-12.3256628518316,56.0416666666667,46.));
#15840=CARTESIAN_POINT('Ctrl Pts',(-23.,55.8333333333333,39.8371685740842));
#15841=CARTESIAN_POINT('Ctrl Pts',(-33.6743371481683,55.625,33.6743371481684));
#15842=CARTESIAN_POINT('Ctrl Pts',(-39.8371685740842,55.4166666666667,23.));
#15843=CARTESIAN_POINT('Ctrl Pts',(-46.,55.2083333333333,12.3256628518317));
#15844=CARTESIAN_POINT('Ctrl Pts',(-46.,55.,0.));
#15845=CARTESIAN_POINT('Ctrl Pts',(-46.,54.7916666666667,-12.3256628518316));
#15846=CARTESIAN_POINT('Ctrl Pts',(-39.8371685740842,54.5833333333333,-23.));
#15847=CARTESIAN_POINT('Ctrl Pts',(-33.6743371481684,54.375,-33.6743371481684));
#15848=CARTESIAN_POINT('Ctrl Pts',(-23.,54.1666666666667,-39.8371685740842));
#15849=CARTESIAN_POINT('Ctrl Pts',(-12.3256628518317,53.9583333333333,-46.));
#15850=CARTESIAN_POINT('Ctrl Pts',(-2.81668763803891E-15,53.75,-46.));
#15851=CARTESIAN_POINT('Ctrl Pts',(12.3256628518316,53.5416666666667,-46.));
#15852=CARTESIAN_POINT('Ctrl Pts',(23.,53.3333333333333,-39.8371685740842));
#15853=CARTESIAN_POINT('Ctrl Pts',(33.6743371481683,53.125,-33.6743371481684));
#15854=CARTESIAN_POINT('Ctrl Pts',(39.8371685740842,52.9166666666667,-23.));
#15855=CARTESIAN_POINT('Ctrl Pts',(46.,52.7083333333333,-12.3256628518317));
#15856=CARTESIAN_POINT('Ctrl Pts',(46.,52.5,-5.63337527607782E-15));
#15857=CARTESIAN_POINT('Ctrl Pts',(46.,52.2916666666667,12.3256628518316));
#15858=CARTESIAN_POINT('Ctrl Pts',(39.8371685740842,52.0833333333333,23.));
#15859=CARTESIAN_POINT('Ctrl Pts',(33.6743371481684,51.875,33.6743371481683));
#15860=CARTESIAN_POINT('Ctrl Pts',(23.,51.6666666666667,39.8371685740842));
#15861=CARTESIAN_POINT('Ctrl Pts',(12.3256628518317,51.4583333333333,46.));
#15862=CARTESIAN_POINT('Ctrl Pts',(8.45006291411674E-15,51.25,46.));
#15863=CARTESIAN_POINT('Ctrl Pts',(-12.3256628518316,51.0416666666667,46.));
#15864=CARTESIAN_POINT('Ctrl Pts',(-23.,50.8333333333333,39.8371685740842));
#15865=CARTESIAN_POINT('Ctrl Pts',(-33.6743371481683,50.625,33.6743371481684));
#15866=CARTESIAN_POINT('Ctrl Pts',(-39.8371685740842,50.4166666666667,23.));
#15867=CARTESIAN_POINT('Ctrl Pts',(-46.,50.2083333333333,12.3256628518317));
#15868=CARTESIAN_POINT('Ctrl Pts',(-46.,50.,0.));
#15869=CARTESIAN_POINT('Ctrl Pts',(-46.,49.7916666666667,-12.3256628518316));
#15870=CARTESIAN_POINT('Ctrl Pts',(-39.8371685740842,49.5833333333333,-23.));
#15871=CARTESIAN_POINT('Ctrl Pts',(-33.6743371481684,49.375,-33.6743371481684));
#15872=CARTESIAN_POINT('Ctrl Pts',(-23.,49.1666666666667,-39.8371685740842));
#15873=CARTESIAN_POINT('Ctrl Pts',(-12.3256628518317,48.9583333333333,-46.));
#15874=CARTESIAN_POINT('Ctrl Pts',(-2.81668763803891E-15,48.75,-46.));
#15875=CARTESIAN_POINT('Ctrl Pts',(12.3256628518316,48.5416666666667,-46.));
#15876=CARTESIAN_POINT('Ctrl Pts',(23.,48.3333333333333,-39.8371685740842));
#15877=CARTESIAN_POINT('Ctrl Pts',(33.6743371481683,48.125,-33.6743371481684));
#15878=CARTESIAN_POINT('Ctrl Pts',(39.8371685740842,47.9166666666667,-23.));
#15879=CARTESIAN_POINT('Ctrl Pts',(46.,47.7083333333333,-12.3256628518317));
#15880=CARTESIAN_POINT('Ctrl Pts',(46.,47.5,-5.63337527607782E-15));
#15881=CARTESIAN_POINT('Ctrl Pts',(46.,47.2916666666667,12.3256628518316));
#15882=CARTESIAN_POINT('Ctrl Pts',(39.8371685740842,47.0833333333333,23.));
#15883=CARTESIAN_POINT('Ctrl Pts',(33.6743371481684,46.875,33.6743371481683));
#15884=CARTESIAN_POINT('Ctrl Pts',(23.,46.6666666666667,39.8371685740842));
#15885=CARTESIAN_POINT('Ctrl Pts',(12.3256628518317,46.4583333333333,46.));
#15886=CARTESIAN_POINT('Ctrl Pts',(8.45006291411674E-15,46.25,46.));
#15887=CARTESIAN_POINT('Ctrl Pts',(-12.3256628518316,46.0416666666667,46.));
#15888=CARTESIAN_POINT('Ctrl Pts',(-23.,45.8333333333333,39.8371685740842));
#15889=CARTESIAN_POINT('Ctrl Pts',(-33.6743371481683,45.625,33.6743371481684));
#15890=CARTESIAN_POINT('Ctrl Pts',(-39.8371685740842,45.4166666666667,23.));
#15891=CARTESIAN_POINT('Ctrl Pts',(-46.,45.2083333333333,12.3256628518317));
#15892=CARTESIAN_POINT('Ctrl Pts',(-46.,45.,0.));
#15893=CARTESIAN_POINT('Ctrl Pts',(-46.,44.7916666666667,-12.3256628518316));
#15894=CARTESIAN_POINT('Ctrl Pts',(-39.8371685740842,44.5833333333333,-23.));
#15895=CARTESIAN_POINT('Ctrl Pts',(-33.6743371481684,44.375,-33.6743371481684));
#15896=CARTESIAN_POINT('Ctrl Pts',(-23.,44.1666666666667,-39.8371685740842));
#15897=CARTESIAN_POINT('Ctrl Pts',(-12.3256628518317,43.9583333333333,-46.));
#15898=CARTESIAN_POINT('Ctrl Pts',(-2.81668763803891E-15,43.75,-46.));
#15899=CARTESIAN_POINT('Ctrl Pts',(12.3256628518316,43.5416666666667,-46.));
#15900=CARTESIAN_POINT('Ctrl Pts',(23.,43.3333333333333,-39.8371685740842));
#15901=CARTESIAN_POINT('Ctrl Pts',(33.6743371481683,43.125,-33.6743371481684));
#15902=CARTESIAN_POINT('Ctrl Pts',(39.8371685740842,42.9166666666667,-23.));
#15903=CARTESIAN_POINT('Ctrl Pts',(46.,42.7083333333333,-12.3256628518317));
#15904=CARTESIAN_POINT('Ctrl Pts',(46.,42.5,-5.63337527607782E-15));
#15905=CARTESIAN_POINT('Ctrl Pts',(46.,42.2916666666667,12.3256628518316));
#15906=CARTESIAN_POINT('Ctrl Pts',(39.8371685740842,42.0833333333333,23.));
#15907=CARTESIAN_POINT('Ctrl Pts',(33.6743371481684,41.875,33.6743371481683));
#15908=CARTESIAN_POINT('Ctrl Pts',(23.,41.6666666666667,39.8371685740842));
#15909=CARTESIAN_POINT('Ctrl Pts',(12.3256628518317,41.4583333333333,46.));
#15910=CARTESIAN_POINT('Ctrl Pts',(8.45006291411674E-15,41.25,46.));
#15911=CARTESIAN_POINT('Ctrl Pts',(-12.3256628518316,41.0416666666667,46.));
#15912=CARTESIAN_POINT('Ctrl Pts',(-23.,40.8333333333333,39.8371685740842));
#15913=CARTESIAN_POINT('Ctrl Pts',(-33.6743371481683,40.625,33.6743371481684));
#15914=CARTESIAN_POINT('Ctrl Pts',(-39.8371685740842,40.4166666666667,23.));
#15915=CARTESIAN_POINT('Ctrl Pts',(-46.,40.2083333333333,12.3256628518317));
#15916=CARTESIAN_POINT('Ctrl Pts',(-46.,40.,0.));
#15917=CARTESIAN_POINT('Ctrl Pts',(-46.,39.7916666666667,-12.3256628518316));
#15918=CARTESIAN_POINT('Ctrl Pts',(-39.8371685740842,39.5833333333333,-23.));
#15919=CARTESIAN_POINT('Ctrl Pts',(-33.6743371481684,39.375,-33.6743371481684));
#15920=CARTESIAN_POINT('Ctrl Pts',(-23.,39.1666666666667,-39.8371685740842));
#15921=CARTESIAN_POINT('Ctrl Pts',(-12.3256628518317,38.9583333333333,-46.));
#15922=CARTESIAN_POINT('Ctrl Pts',(-2.81668763803891E-15,38.75,-46.));
#15923=CARTESIAN_POINT('Ctrl Pts',(12.3256628518316,38.5416666666667,-46.));
#15924=CARTESIAN_POINT('Ctrl Pts',(23.,38.3333333333333,-39.8371685740842));
#15925=CARTESIAN_POINT('Ctrl Pts',(33.6743371481683,38.125,-33.6743371481684));
#15926=CARTESIAN_POINT('Ctrl Pts',(39.8371685740842,37.9166666666667,-23.));
#15927=CARTESIAN_POINT('Ctrl Pts',(46.,37.7083333333333,-12.3256628518317));
#15928=CARTESIAN_POINT('Ctrl Pts',(46.,37.5,-5.63337527607782E-15));
#15929=CARTESIAN_POINT('Ctrl Pts',(46.,37.2916666666667,12.3256628518316));
#15930=CARTESIAN_POINT('Ctrl Pts',(39.8371685740842,37.0833333333333,23.));
#15931=CARTESIAN_POINT('Ctrl Pts',(33.6743371481684,36.875,33.6743371481683));
#15932=CARTESIAN_POINT('Ctrl Pts',(23.,36.6666666666667,39.8371685740842));
#15933=CARTESIAN_POINT('Ctrl Pts',(12.3256628518317,36.4583333333333,46.));
#15934=CARTESIAN_POINT('Ctrl Pts',(8.45006291411674E-15,36.25,46.));
#15935=CARTESIAN_POINT('Ctrl Pts',(-12.3256628518316,36.0416666666667,46.));
#15936=CARTESIAN_POINT('Ctrl Pts',(-23.,35.8333333333333,39.8371685740842));
#15937=CARTESIAN_POINT('Ctrl Pts',(-33.6743371481683,35.625,33.6743371481684));
#15938=CARTESIAN_POINT('Ctrl Pts',(-39.8371685740842,35.4166666666667,23.));
#15939=CARTESIAN_POINT('Ctrl Pts',(-46.,35.2083333333333,12.3256628518317));
#15940=CARTESIAN_POINT('Ctrl Pts',(-46.,35.,0.));
#15941=CARTESIAN_POINT('Ctrl Pts',(-46.,34.7916666666667,-12.3256628518316));
#15942=CARTESIAN_POINT('Ctrl Pts',(-39.8371685740842,34.5833333333333,-23.));
#15943=CARTESIAN_POINT('Ctrl Pts',(-33.6743371481684,34.375,-33.6743371481684));
#15944=CARTESIAN_POINT('Ctrl Pts',(-23.,34.1666666666667,-39.8371685740842));
#15945=CARTESIAN_POINT('Ctrl Pts',(-12.3256628518317,33.9583333333333,-46.));
#15946=CARTESIAN_POINT('Ctrl Pts',(-2.81668763803891E-15,33.75,-46.));
#15947=CARTESIAN_POINT('Ctrl Pts',(12.3256628518316,33.5416666666667,-46.));
#15948=CARTESIAN_POINT('Ctrl Pts',(23.,33.3333333333333,-39.8371685740842));
#15949=CARTESIAN_POINT('Ctrl Pts',(33.6743371481683,33.125,-33.6743371481684));
#15950=CARTESIAN_POINT('Ctrl Pts',(39.8371685740842,32.9166666666667,-23.));
#15951=CARTESIAN_POINT('Ctrl Pts',(46.,32.7083333333333,-12.3256628518317));
#15952=CARTESIAN_POINT('Ctrl Pts',(46.,32.5,-5.63337527607782E-15));
#15953=CARTESIAN_POINT('Ctrl Pts',(46.,32.2916666666667,12.3256628518316));
#15954=CARTESIAN_POINT('Ctrl Pts',(39.8371685740842,32.0833333333333,23.));
#15955=CARTESIAN_POINT('Ctrl Pts',(33.6743371481684,31.875,33.6743371481683));
#15956=CARTESIAN_POINT('Ctrl Pts',(23.,31.6666666666667,39.8371685740842));
#15957=CARTESIAN_POINT('Ctrl Pts',(12.3256628518317,31.4583333333333,46.));
#15958=CARTESIAN_POINT('Ctrl Pts',(8.45006291411674E-15,31.25,46.));
#15959=CARTESIAN_POINT('Ctrl Pts',(-12.3256628518316,31.0416666666667,46.));
#15960=CARTESIAN_POINT('Ctrl Pts',(-23.,30.8333333333333,39.8371685740842));
#15961=CARTESIAN_POINT('Ctrl Pts',(-33.6743371481683,30.625,33.6743371481684));
#15962=CARTESIAN_POINT('Ctrl Pts',(-39.8371685740842,30.4166666666667,23.));
#15963=CARTESIAN_POINT('Ctrl Pts',(-46.,30.2083333333333,12.3256628518317));
#15964=CARTESIAN_POINT('Ctrl Pts',(-46.,30.,0.));
#15965=CARTESIAN_POINT('Origin',(4513.80899817375,-7915.1585511582,-4.33049284435178));
#15966=CARTESIAN_POINT('Ctrl Pts',(-4.32456003949879,38.8240181593937,-45.7962681936506));
#15967=CARTESIAN_POINT('Ctrl Pts',(-4.32456003949872,38.6905125468623,-46.0278818021281));
#15968=CARTESIAN_POINT('Ctrl Pts',(-4.32456003949878,38.4234964717135,-46.4911062234486));
#15969=CARTESIAN_POINT('Ctrl Pts',(-4.32456003949881,38.1564711191154,-46.954325296818));
#15970=CARTESIAN_POINT('Ctrl Pts',(-4.32456003949881,37.7677643029224,-47.6286149142205));
#15971=CARTESIAN_POINT('Ctrl Pts',(-4.32456003949869,37.5125642776457,-48.0712916022845));
#15972=CARTESIAN_POINT('Ctrl Pts',(-4.32456003949869,37.2573567866782,-48.5139639861634));
#15973=CARTESIAN_POINT('Ctrl Pts',(-48.706329375,58.437500006828,-1.8898197019151E-14));
#15974=CARTESIAN_POINT('Ctrl Pts',(-48.706329375,58.2291666734946,-13.0508216223155));
#15975=CARTESIAN_POINT('Ctrl Pts',(-42.1809185638422,58.0208333401613,-24.3531646875));
#15976=CARTESIAN_POINT('Ctrl Pts',(-35.6555077526845,57.812500006828,-35.6555077526845));
#15977=CARTESIAN_POINT('Ctrl Pts',(-24.3531646875,57.6041666734946,-42.1809185638422));
#15978=CARTESIAN_POINT('Ctrl Pts',(-13.0508216223155,57.3958333401613,-48.706329375));
#15979=CARTESIAN_POINT('Ctrl Pts',(1.59157945007855E-14,57.187500006828,
-48.706329375));
#15980=CARTESIAN_POINT('Ctrl Pts',(13.0508216223155,56.9791666734946,-48.706329375));
#15981=CARTESIAN_POINT('Ctrl Pts',(24.3531646875,56.7708333401613,-42.1809185638422));
#15982=CARTESIAN_POINT('Ctrl Pts',(35.6555077526845,56.562500006828,-35.6555077526845));
#15983=CARTESIAN_POINT('Ctrl Pts',(42.1809185638422,56.3541666734946,-24.3531646875));
#15984=CARTESIAN_POINT('Ctrl Pts',(48.706329375,56.1458333401613,-13.0508216223155));
#15985=CARTESIAN_POINT('Ctrl Pts',(48.706329375,55.937500006828,1.293339198242E-14));
#15986=CARTESIAN_POINT('Ctrl Pts',(48.706329375,55.7291666734946,13.0508216223155));
#15987=CARTESIAN_POINT('Ctrl Pts',(42.1809185638422,55.5208333401613,24.3531646875));
#15988=CARTESIAN_POINT('Ctrl Pts',(35.6555077526845,55.312500006828,35.6555077526845));
#15989=CARTESIAN_POINT('Ctrl Pts',(24.3531646875,55.1041666734946,42.1809185638422));
#15990=CARTESIAN_POINT('Ctrl Pts',(13.0508216223155,54.8958333401613,48.706329375));
#15991=CARTESIAN_POINT('Ctrl Pts',(-9.95098946405443E-15,54.687500006828,
48.706329375));
#15992=CARTESIAN_POINT('Ctrl Pts',(-13.0508216223155,54.4791666734946,48.706329375));
#15993=CARTESIAN_POINT('Ctrl Pts',(-24.3531646875,54.2708333401613,42.1809185638423));
#15994=CARTESIAN_POINT('Ctrl Pts',(-35.6555077526845,54.062500006828,35.6555077526845));
#15995=CARTESIAN_POINT('Ctrl Pts',(-42.1809185638422,53.8541666734946,24.3531646875));
#15996=CARTESIAN_POINT('Ctrl Pts',(-48.706329375,53.6458333401613,13.0508216223155));
#15997=CARTESIAN_POINT('Ctrl Pts',(-48.706329375,53.437500006828,-1.8898197019151E-14));
#15998=CARTESIAN_POINT('Ctrl Pts',(-48.706329375,53.2291666734946,-13.0508216223155));
#15999=CARTESIAN_POINT('Ctrl Pts',(-42.1809185638422,53.0208333401613,-24.3531646875));
#16000=CARTESIAN_POINT('Ctrl Pts',(-35.6555077526845,52.812500006828,-35.6555077526845));
#16001=CARTESIAN_POINT('Ctrl Pts',(-24.3531646875,52.6041666734946,-42.1809185638422));
#16002=CARTESIAN_POINT('Ctrl Pts',(-13.0508216223155,52.3958333401613,-48.706329375));
#16003=CARTESIAN_POINT('Ctrl Pts',(1.59157945007855E-14,52.187500006828,
-48.706329375));
#16004=CARTESIAN_POINT('Ctrl Pts',(13.0508216223155,51.9791666734946,-48.706329375));
#16005=CARTESIAN_POINT('Ctrl Pts',(24.3531646875,51.7708333401613,-42.1809185638422));
#16006=CARTESIAN_POINT('Ctrl Pts',(35.6555077526845,51.562500006828,-35.6555077526845));
#16007=CARTESIAN_POINT('Ctrl Pts',(42.1809185638422,51.3541666734946,-24.3531646875));
#16008=CARTESIAN_POINT('Ctrl Pts',(48.706329375,51.1458333401613,-13.0508216223155));
#16009=CARTESIAN_POINT('Ctrl Pts',(48.706329375,50.937500006828,1.293339198242E-14));
#16010=CARTESIAN_POINT('Ctrl Pts',(48.706329375,50.7291666734946,13.0508216223155));
#16011=CARTESIAN_POINT('Ctrl Pts',(42.1809185638422,50.5208333401613,24.3531646875));
#16012=CARTESIAN_POINT('Ctrl Pts',(35.6555077526845,50.312500006828,35.6555077526845));
#16013=CARTESIAN_POINT('Ctrl Pts',(24.3531646875,50.1041666734946,42.1809185638422));
#16014=CARTESIAN_POINT('Ctrl Pts',(13.0508216223155,49.8958333401613,48.706329375));
#16015=CARTESIAN_POINT('Ctrl Pts',(-9.95098946405443E-15,49.687500006828,
48.706329375));
#16016=CARTESIAN_POINT('Ctrl Pts',(-13.0508216223155,49.4791666734946,48.706329375));
#16017=CARTESIAN_POINT('Ctrl Pts',(-24.3531646875,49.2708333401613,42.1809185638423));
#16018=CARTESIAN_POINT('Ctrl Pts',(-35.6555077526845,49.062500006828,35.6555077526845));
#16019=CARTESIAN_POINT('Ctrl Pts',(-42.1809185638422,48.8541666734946,24.3531646875));
#16020=CARTESIAN_POINT('Ctrl Pts',(-48.706329375,48.6458333401613,13.0508216223155));
#16021=CARTESIAN_POINT('Ctrl Pts',(-48.706329375,48.437500006828,-1.8898197019151E-14));
#16022=CARTESIAN_POINT('Ctrl Pts',(-48.706329375,48.2291666734946,-13.0508216223155));
#16023=CARTESIAN_POINT('Ctrl Pts',(-42.1809185638422,48.0208333401613,-24.3531646875));
#16024=CARTESIAN_POINT('Ctrl Pts',(-35.6555077526845,47.812500006828,-35.6555077526845));
#16025=CARTESIAN_POINT('Ctrl Pts',(-24.3531646875,47.6041666734946,-42.1809185638422));
#16026=CARTESIAN_POINT('Ctrl Pts',(-13.0508216223155,47.3958333401613,-48.706329375));
#16027=CARTESIAN_POINT('Ctrl Pts',(1.59157945007855E-14,47.187500006828,
-48.706329375));
#16028=CARTESIAN_POINT('Ctrl Pts',(13.0508216223155,46.9791666734946,-48.706329375));
#16029=CARTESIAN_POINT('Ctrl Pts',(24.3531646875,46.7708333401613,-42.1809185638422));
#16030=CARTESIAN_POINT('Ctrl Pts',(35.6555077526845,46.562500006828,-35.6555077526845));
#16031=CARTESIAN_POINT('Ctrl Pts',(42.1809185638422,46.3541666734946,-24.3531646875));
#16032=CARTESIAN_POINT('Ctrl Pts',(48.706329375,46.1458333401613,-13.0508216223155));
#16033=CARTESIAN_POINT('Ctrl Pts',(48.706329375,45.937500006828,1.293339198242E-14));
#16034=CARTESIAN_POINT('Ctrl Pts',(48.706329375,45.7291666734946,13.0508216223155));
#16035=CARTESIAN_POINT('Ctrl Pts',(42.1809185638422,45.5208333401613,24.3531646875));
#16036=CARTESIAN_POINT('Ctrl Pts',(35.6555077526845,45.312500006828,35.6555077526845));
#16037=CARTESIAN_POINT('Ctrl Pts',(24.3531646875,45.1041666734946,42.1809185638422));
#16038=CARTESIAN_POINT('Ctrl Pts',(13.0508216223155,44.8958333401613,48.706329375));
#16039=CARTESIAN_POINT('Ctrl Pts',(-9.95098946405443E-15,44.687500006828,
48.706329375));
#16040=CARTESIAN_POINT('Ctrl Pts',(-13.0508216223155,44.4791666734946,48.706329375));
#16041=CARTESIAN_POINT('Ctrl Pts',(-24.3531646875,44.2708333401613,42.1809185638423));
#16042=CARTESIAN_POINT('Ctrl Pts',(-35.6555077526845,44.062500006828,35.6555077526845));
#16043=CARTESIAN_POINT('Ctrl Pts',(-42.1809185638422,43.8541666734946,24.3531646875));
#16044=CARTESIAN_POINT('Ctrl Pts',(-48.706329375,43.6458333401613,13.0508216223155));
#16045=CARTESIAN_POINT('Ctrl Pts',(-48.706329375,43.437500006828,-1.8898197019151E-14));
#16046=CARTESIAN_POINT('Ctrl Pts',(-48.706329375,43.2291666734946,-13.0508216223155));
#16047=CARTESIAN_POINT('Ctrl Pts',(-42.1809185638422,43.0208333401613,-24.3531646875));
#16048=CARTESIAN_POINT('Ctrl Pts',(-35.6555077526845,42.812500006828,-35.6555077526845));
#16049=CARTESIAN_POINT('Ctrl Pts',(-24.3531646875,42.6041666734946,-42.1809185638422));
#16050=CARTESIAN_POINT('Ctrl Pts',(-13.0508216223155,42.3958333401613,-48.706329375));
#16051=CARTESIAN_POINT('Ctrl Pts',(1.59157945007855E-14,42.187500006828,
-48.706329375));
#16052=CARTESIAN_POINT('Ctrl Pts',(13.0508216223155,41.9791666734946,-48.706329375));
#16053=CARTESIAN_POINT('Ctrl Pts',(24.3531646875,41.7708333401613,-42.1809185638422));
#16054=CARTESIAN_POINT('Ctrl Pts',(35.6555077526845,41.562500006828,-35.6555077526845));
#16055=CARTESIAN_POINT('Ctrl Pts',(42.1809185638422,41.3541666734946,-24.3531646875));
#16056=CARTESIAN_POINT('Ctrl Pts',(48.706329375,41.1458333401613,-13.0508216223155));
#16057=CARTESIAN_POINT('Ctrl Pts',(48.706329375,40.937500006828,1.293339198242E-14));
#16058=CARTESIAN_POINT('Ctrl Pts',(48.706329375,40.7291666734946,13.0508216223155));
#16059=CARTESIAN_POINT('Ctrl Pts',(42.1809185638422,40.5208333401613,24.3531646875));
#16060=CARTESIAN_POINT('Ctrl Pts',(35.6555077526845,40.312500006828,35.6555077526845));
#16061=CARTESIAN_POINT('Ctrl Pts',(24.3531646875,40.1041666734946,42.1809185638422));
#16062=CARTESIAN_POINT('Ctrl Pts',(13.0508216223155,39.8958333401613,48.706329375));
#16063=CARTESIAN_POINT('Ctrl Pts',(-9.95098946405443E-15,39.687500006828,
48.706329375));
#16064=CARTESIAN_POINT('Ctrl Pts',(-13.0508216223155,39.4791666734946,48.706329375));
#16065=CARTESIAN_POINT('Ctrl Pts',(-24.3531646875,39.2708333401613,42.1809185638423));
#16066=CARTESIAN_POINT('Ctrl Pts',(-35.6555077526845,39.062500006828,35.6555077526845));
#16067=CARTESIAN_POINT('Ctrl Pts',(-42.1809185638422,38.8541666734946,24.3531646875));
#16068=CARTESIAN_POINT('Ctrl Pts',(-48.706329375,38.6458333401613,13.0508216223155));
#16069=CARTESIAN_POINT('Ctrl Pts',(-48.706329375,38.437500006828,-1.8898197019151E-14));
#16070=CARTESIAN_POINT('Ctrl Pts',(-48.706329375,38.2291666734946,-13.0508216223155));
#16071=CARTESIAN_POINT('Ctrl Pts',(-42.1809185638422,38.0208333401613,-24.3531646875));
#16072=CARTESIAN_POINT('Ctrl Pts',(-35.6555077526845,37.812500006828,-35.6555077526845));
#16073=CARTESIAN_POINT('Ctrl Pts',(-24.3531646875,37.6041666734946,-42.1809185638422));
#16074=CARTESIAN_POINT('Ctrl Pts',(-13.0508216223155,37.3958333401613,-48.706329375));
#16075=CARTESIAN_POINT('Ctrl Pts',(1.59157945007855E-14,37.187500006828,
-48.706329375));
#16076=CARTESIAN_POINT('Ctrl Pts',(13.0508216223155,36.9791666734946,-48.706329375));
#16077=CARTESIAN_POINT('Ctrl Pts',(24.3531646875,36.7708333401613,-42.1809185638422));
#16078=CARTESIAN_POINT('Ctrl Pts',(35.6555077526845,36.562500006828,-35.6555077526845));
#16079=CARTESIAN_POINT('Ctrl Pts',(42.1809185638422,36.3541666734946,-24.3531646875));
#16080=CARTESIAN_POINT('Ctrl Pts',(48.706329375,36.1458333401613,-13.0508216223155));
#16081=CARTESIAN_POINT('Ctrl Pts',(48.706329375,35.937500006828,1.293339198242E-14));
#16082=CARTESIAN_POINT('Ctrl Pts',(48.706329375,35.7291666734946,13.0508216223155));
#16083=CARTESIAN_POINT('Ctrl Pts',(42.1809185638422,35.5208333401613,24.3531646875));
#16084=CARTESIAN_POINT('Ctrl Pts',(35.6555077526845,35.312500006828,35.6555077526845));
#16085=CARTESIAN_POINT('Ctrl Pts',(24.3531646875,35.1041666734946,42.1809185638422));
#16086=CARTESIAN_POINT('Ctrl Pts',(13.0508216223155,34.8958333401613,48.706329375));
#16087=CARTESIAN_POINT('Ctrl Pts',(-9.95098946405443E-15,34.687500006828,
48.706329375));
#16088=CARTESIAN_POINT('Ctrl Pts',(-13.0508216223155,34.4791666734946,48.706329375));
#16089=CARTESIAN_POINT('Ctrl Pts',(-24.3531646875,34.2708333401613,42.1809185638423));
#16090=CARTESIAN_POINT('Ctrl Pts',(-35.6555077526845,34.062500006828,35.6555077526845));
#16091=CARTESIAN_POINT('Ctrl Pts',(-42.1809185638422,33.8541666734946,24.3531646875));
#16092=CARTESIAN_POINT('Ctrl Pts',(-48.706329375,33.6458333401613,13.0508216223155));
#16093=CARTESIAN_POINT('Ctrl Pts',(-48.706329375,33.437500006828,-1.8898197019151E-14));
#16094=CARTESIAN_POINT('Ctrl Pts',(-48.706329375,33.2291666734946,-13.0508216223155));
#16095=CARTESIAN_POINT('Ctrl Pts',(-42.1809185638422,33.0208333401613,-24.3531646875));
#16096=CARTESIAN_POINT('Ctrl Pts',(-35.6555077526845,32.812500006828,-35.6555077526845));
#16097=CARTESIAN_POINT('Ctrl Pts',(-24.3531646875,32.6041666734946,-42.1809185638422));
#16098=CARTESIAN_POINT('Ctrl Pts',(-13.0508216223155,32.3958333401613,-48.706329375));
#16099=CARTESIAN_POINT('Ctrl Pts',(1.59157945007855E-14,32.187500006828,
-48.706329375));
#16100=CARTESIAN_POINT('Ctrl Pts',(13.0508216223155,31.9791666734946,-48.706329375));
#16101=CARTESIAN_POINT('Ctrl Pts',(24.3531646875,31.7708333401613,-42.1809185638422));
#16102=CARTESIAN_POINT('Ctrl Pts',(35.6555077526845,31.562500006828,-35.6555077526845));
#16103=CARTESIAN_POINT('Ctrl Pts',(42.1809185638422,31.3541666734946,-24.3531646875));
#16104=CARTESIAN_POINT('Ctrl Pts',(48.706329375,31.1458333401613,-13.0508216223155));
#16105=CARTESIAN_POINT('Ctrl Pts',(48.706329375,30.937500006828,1.293339198242E-14));
#16106=CARTESIAN_POINT('Ctrl Pts',(48.706329375,30.7291666734946,13.0508216223155));
#16107=CARTESIAN_POINT('Ctrl Pts',(42.1809185638422,30.5208333401613,24.3531646875));
#16108=CARTESIAN_POINT('Ctrl Pts',(35.6555077526845,30.312500006828,35.6555077526845));
#16109=CARTESIAN_POINT('Ctrl Pts',(24.3531646875,30.1041666734946,42.1809185638422));
#16110=CARTESIAN_POINT('Ctrl Pts',(13.0508216223155,29.8958333401613,48.706329375));
#16111=CARTESIAN_POINT('Ctrl Pts',(-9.95098946405443E-15,29.687500006828,
48.706329375));
#16112=CARTESIAN_POINT('Ctrl Pts',(-13.0508216223155,29.4791666734946,48.706329375));
#16113=CARTESIAN_POINT('Ctrl Pts',(-24.3531646875,29.2708333401613,42.1809185638423));
#16114=CARTESIAN_POINT('Ctrl Pts',(-35.6555077526845,29.062500006828,35.6555077526845));
#16115=CARTESIAN_POINT('Ctrl Pts',(-42.1809185638422,28.8541666734946,24.3531646875));
#16116=CARTESIAN_POINT('Ctrl Pts',(-48.706329375,28.6458333401613,13.0508216223155));
#16117=CARTESIAN_POINT('Ctrl Pts',(-48.706329375,28.437500006828,-1.8898197019151E-14));
#16118=CARTESIAN_POINT('Ctrl Pts',(-46.,60.,0.));
#16119=CARTESIAN_POINT('Ctrl Pts',(-46.,59.7916666666667,-12.3256628518316));
#16120=CARTESIAN_POINT('Ctrl Pts',(-39.8371685740842,59.5833333333333,-23.));
#16121=CARTESIAN_POINT('Ctrl Pts',(-33.6743371481684,59.375,-33.6743371481684));
#16122=CARTESIAN_POINT('Ctrl Pts',(-23.,59.1666666666667,-39.8371685740842));
#16123=CARTESIAN_POINT('Ctrl Pts',(-12.3256628518317,58.9583333333333,-46.));
#16124=CARTESIAN_POINT('Ctrl Pts',(-2.81668763803891E-15,58.75,-46.));
#16125=CARTESIAN_POINT('Ctrl Pts',(12.3256628518316,58.5416666666667,-46.));
#16126=CARTESIAN_POINT('Ctrl Pts',(23.,58.3333333333333,-39.8371685740842));
#16127=CARTESIAN_POINT('Ctrl Pts',(33.6743371481683,58.125,-33.6743371481684));
#16128=CARTESIAN_POINT('Ctrl Pts',(39.8371685740842,57.9166666666667,-23.));
#16129=CARTESIAN_POINT('Ctrl Pts',(46.,57.7083333333333,-12.3256628518317));
#16130=CARTESIAN_POINT('Ctrl Pts',(46.,57.5,-5.63337527607782E-15));
#16131=CARTESIAN_POINT('Ctrl Pts',(46.,57.2916666666667,12.3256628518316));
#16132=CARTESIAN_POINT('Ctrl Pts',(39.8371685740842,57.0833333333333,23.));
#16133=CARTESIAN_POINT('Ctrl Pts',(33.6743371481684,56.875,33.6743371481683));
#16134=CARTESIAN_POINT('Ctrl Pts',(23.,56.6666666666667,39.8371685740842));
#16135=CARTESIAN_POINT('Ctrl Pts',(12.3256628518317,56.4583333333333,46.));
#16136=CARTESIAN_POINT('Ctrl Pts',(8.45006291411674E-15,56.25,46.));
#16137=CARTESIAN_POINT('Ctrl Pts',(-12.3256628518316,56.0416666666667,46.));
#16138=CARTESIAN_POINT('Ctrl Pts',(-23.,55.8333333333333,39.8371685740842));
#16139=CARTESIAN_POINT('Ctrl Pts',(-33.6743371481683,55.625,33.6743371481684));
#16140=CARTESIAN_POINT('Ctrl Pts',(-39.8371685740842,55.4166666666667,23.));
#16141=CARTESIAN_POINT('Ctrl Pts',(-46.,55.2083333333333,12.3256628518317));
#16142=CARTESIAN_POINT('Ctrl Pts',(-46.,55.,0.));
#16143=CARTESIAN_POINT('Ctrl Pts',(-46.,54.7916666666667,-12.3256628518316));
#16144=CARTESIAN_POINT('Ctrl Pts',(-39.8371685740842,54.5833333333333,-23.));
#16145=CARTESIAN_POINT('Ctrl Pts',(-33.6743371481684,54.375,-33.6743371481684));
#16146=CARTESIAN_POINT('Ctrl Pts',(-23.,54.1666666666667,-39.8371685740842));
#16147=CARTESIAN_POINT('Ctrl Pts',(-12.3256628518317,53.9583333333333,-46.));
#16148=CARTESIAN_POINT('Ctrl Pts',(-2.81668763803891E-15,53.75,-46.));
#16149=CARTESIAN_POINT('Ctrl Pts',(12.3256628518316,53.5416666666667,-46.));
#16150=CARTESIAN_POINT('Ctrl Pts',(23.,53.3333333333333,-39.8371685740842));
#16151=CARTESIAN_POINT('Ctrl Pts',(33.6743371481683,53.125,-33.6743371481684));
#16152=CARTESIAN_POINT('Ctrl Pts',(39.8371685740842,52.9166666666667,-23.));
#16153=CARTESIAN_POINT('Ctrl Pts',(46.,52.7083333333333,-12.3256628518317));
#16154=CARTESIAN_POINT('Ctrl Pts',(46.,52.5,-5.63337527607782E-15));
#16155=CARTESIAN_POINT('Ctrl Pts',(46.,52.2916666666667,12.3256628518316));
#16156=CARTESIAN_POINT('Ctrl Pts',(39.8371685740842,52.0833333333333,23.));
#16157=CARTESIAN_POINT('Ctrl Pts',(33.6743371481684,51.875,33.6743371481683));
#16158=CARTESIAN_POINT('Ctrl Pts',(23.,51.6666666666667,39.8371685740842));
#16159=CARTESIAN_POINT('Ctrl Pts',(12.3256628518317,51.4583333333333,46.));
#16160=CARTESIAN_POINT('Ctrl Pts',(8.45006291411674E-15,51.25,46.));
#16161=CARTESIAN_POINT('Ctrl Pts',(-12.3256628518316,51.0416666666667,46.));
#16162=CARTESIAN_POINT('Ctrl Pts',(-23.,50.8333333333333,39.8371685740842));
#16163=CARTESIAN_POINT('Ctrl Pts',(-33.6743371481683,50.625,33.6743371481684));
#16164=CARTESIAN_POINT('Ctrl Pts',(-39.8371685740842,50.4166666666667,23.));
#16165=CARTESIAN_POINT('Ctrl Pts',(-46.,50.2083333333333,12.3256628518317));
#16166=CARTESIAN_POINT('Ctrl Pts',(-46.,50.,0.));
#16167=CARTESIAN_POINT('Ctrl Pts',(-46.,49.7916666666667,-12.3256628518316));
#16168=CARTESIAN_POINT('Ctrl Pts',(-39.8371685740842,49.5833333333333,-23.));
#16169=CARTESIAN_POINT('Ctrl Pts',(-33.6743371481684,49.375,-33.6743371481684));
#16170=CARTESIAN_POINT('Ctrl Pts',(-23.,49.1666666666667,-39.8371685740842));
#16171=CARTESIAN_POINT('Ctrl Pts',(-12.3256628518317,48.9583333333333,-46.));
#16172=CARTESIAN_POINT('Ctrl Pts',(-2.81668763803891E-15,48.75,-46.));
#16173=CARTESIAN_POINT('Ctrl Pts',(12.3256628518316,48.5416666666667,-46.));
#16174=CARTESIAN_POINT('Ctrl Pts',(23.,48.3333333333333,-39.8371685740842));
#16175=CARTESIAN_POINT('Ctrl Pts',(33.6743371481683,48.125,-33.6743371481684));
#16176=CARTESIAN_POINT('Ctrl Pts',(39.8371685740842,47.9166666666667,-23.));
#16177=CARTESIAN_POINT('Ctrl Pts',(46.,47.7083333333333,-12.3256628518317));
#16178=CARTESIAN_POINT('Ctrl Pts',(46.,47.5,-5.63337527607782E-15));
#16179=CARTESIAN_POINT('Ctrl Pts',(46.,47.2916666666667,12.3256628518316));
#16180=CARTESIAN_POINT('Ctrl Pts',(39.8371685740842,47.0833333333333,23.));
#16181=CARTESIAN_POINT('Ctrl Pts',(33.6743371481684,46.875,33.6743371481683));
#16182=CARTESIAN_POINT('Ctrl Pts',(23.,46.6666666666667,39.8371685740842));
#16183=CARTESIAN_POINT('Ctrl Pts',(12.3256628518317,46.4583333333333,46.));
#16184=CARTESIAN_POINT('Ctrl Pts',(8.45006291411674E-15,46.25,46.));
#16185=CARTESIAN_POINT('Ctrl Pts',(-12.3256628518316,46.0416666666667,46.));
#16186=CARTESIAN_POINT('Ctrl Pts',(-23.,45.8333333333333,39.8371685740842));
#16187=CARTESIAN_POINT('Ctrl Pts',(-33.6743371481683,45.625,33.6743371481684));
#16188=CARTESIAN_POINT('Ctrl Pts',(-39.8371685740842,45.4166666666667,23.));
#16189=CARTESIAN_POINT('Ctrl Pts',(-46.,45.2083333333333,12.3256628518317));
#16190=CARTESIAN_POINT('Ctrl Pts',(-46.,45.,0.));
#16191=CARTESIAN_POINT('Ctrl Pts',(-46.,44.7916666666667,-12.3256628518316));
#16192=CARTESIAN_POINT('Ctrl Pts',(-39.8371685740842,44.5833333333333,-23.));
#16193=CARTESIAN_POINT('Ctrl Pts',(-33.6743371481684,44.375,-33.6743371481684));
#16194=CARTESIAN_POINT('Ctrl Pts',(-23.,44.1666666666667,-39.8371685740842));
#16195=CARTESIAN_POINT('Ctrl Pts',(-12.3256628518317,43.9583333333333,-46.));
#16196=CARTESIAN_POINT('Ctrl Pts',(-2.81668763803891E-15,43.75,-46.));
#16197=CARTESIAN_POINT('Ctrl Pts',(12.3256628518316,43.5416666666667,-46.));
#16198=CARTESIAN_POINT('Ctrl Pts',(23.,43.3333333333333,-39.8371685740842));
#16199=CARTESIAN_POINT('Ctrl Pts',(33.6743371481683,43.125,-33.6743371481684));
#16200=CARTESIAN_POINT('Ctrl Pts',(39.8371685740842,42.9166666666667,-23.));
#16201=CARTESIAN_POINT('Ctrl Pts',(46.,42.7083333333333,-12.3256628518317));
#16202=CARTESIAN_POINT('Ctrl Pts',(46.,42.5,-5.63337527607782E-15));
#16203=CARTESIAN_POINT('Ctrl Pts',(46.,42.2916666666667,12.3256628518316));
#16204=CARTESIAN_POINT('Ctrl Pts',(39.8371685740842,42.0833333333333,23.));
#16205=CARTESIAN_POINT('Ctrl Pts',(33.6743371481684,41.875,33.6743371481683));
#16206=CARTESIAN_POINT('Ctrl Pts',(23.,41.6666666666667,39.8371685740842));
#16207=CARTESIAN_POINT('Ctrl Pts',(12.3256628518317,41.4583333333333,46.));
#16208=CARTESIAN_POINT('Ctrl Pts',(8.45006291411674E-15,41.25,46.));
#16209=CARTESIAN_POINT('Ctrl Pts',(-12.3256628518316,41.0416666666667,46.));
#16210=CARTESIAN_POINT('Ctrl Pts',(-23.,40.8333333333333,39.8371685740842));
#16211=CARTESIAN_POINT('Ctrl Pts',(-33.6743371481683,40.625,33.6743371481684));
#16212=CARTESIAN_POINT('Ctrl Pts',(-39.8371685740842,40.4166666666667,23.));
#16213=CARTESIAN_POINT('Ctrl Pts',(-46.,40.2083333333333,12.3256628518317));
#16214=CARTESIAN_POINT('Ctrl Pts',(-46.,40.,0.));
#16215=CARTESIAN_POINT('Ctrl Pts',(-46.,39.7916666666667,-12.3256628518316));
#16216=CARTESIAN_POINT('Ctrl Pts',(-39.8371685740842,39.5833333333333,-23.));
#16217=CARTESIAN_POINT('Ctrl Pts',(-33.6743371481684,39.375,-33.6743371481684));
#16218=CARTESIAN_POINT('Ctrl Pts',(-23.,39.1666666666667,-39.8371685740842));
#16219=CARTESIAN_POINT('Ctrl Pts',(-12.3256628518317,38.9583333333333,-46.));
#16220=CARTESIAN_POINT('Ctrl Pts',(-2.81668763803891E-15,38.75,-46.));
#16221=CARTESIAN_POINT('Ctrl Pts',(12.3256628518316,38.5416666666667,-46.));
#16222=CARTESIAN_POINT('Ctrl Pts',(23.,38.3333333333333,-39.8371685740842));
#16223=CARTESIAN_POINT('Ctrl Pts',(33.6743371481683,38.125,-33.6743371481684));
#16224=CARTESIAN_POINT('Ctrl Pts',(39.8371685740842,37.9166666666667,-23.));
#16225=CARTESIAN_POINT('Ctrl Pts',(46.,37.7083333333333,-12.3256628518317));
#16226=CARTESIAN_POINT('Ctrl Pts',(46.,37.5,-5.63337527607782E-15));
#16227=CARTESIAN_POINT('Ctrl Pts',(46.,37.2916666666667,12.3256628518316));
#16228=CARTESIAN_POINT('Ctrl Pts',(39.8371685740842,37.0833333333333,23.));
#16229=CARTESIAN_POINT('Ctrl Pts',(33.6743371481684,36.875,33.6743371481683));
#16230=CARTESIAN_POINT('Ctrl Pts',(23.,36.6666666666667,39.8371685740842));
#16231=CARTESIAN_POINT('Ctrl Pts',(12.3256628518317,36.4583333333333,46.));
#16232=CARTESIAN_POINT('Ctrl Pts',(8.45006291411674E-15,36.25,46.));
#16233=CARTESIAN_POINT('Ctrl Pts',(-12.3256628518316,36.0416666666667,46.));
#16234=CARTESIAN_POINT('Ctrl Pts',(-23.,35.8333333333333,39.8371685740842));
#16235=CARTESIAN_POINT('Ctrl Pts',(-33.6743371481683,35.625,33.6743371481684));
#16236=CARTESIAN_POINT('Ctrl Pts',(-39.8371685740842,35.4166666666667,23.));
#16237=CARTESIAN_POINT('Ctrl Pts',(-46.,35.2083333333333,12.3256628518317));
#16238=CARTESIAN_POINT('Ctrl Pts',(-46.,35.,0.));
#16239=CARTESIAN_POINT('Ctrl Pts',(-46.,34.7916666666667,-12.3256628518316));
#16240=CARTESIAN_POINT('Ctrl Pts',(-39.8371685740842,34.5833333333333,-23.));
#16241=CARTESIAN_POINT('Ctrl Pts',(-33.6743371481684,34.375,-33.6743371481684));
#16242=CARTESIAN_POINT('Ctrl Pts',(-23.,34.1666666666667,-39.8371685740842));
#16243=CARTESIAN_POINT('Ctrl Pts',(-12.3256628518317,33.9583333333333,-46.));
#16244=CARTESIAN_POINT('Ctrl Pts',(-2.81668763803891E-15,33.75,-46.));
#16245=CARTESIAN_POINT('Ctrl Pts',(12.3256628518316,33.5416666666667,-46.));
#16246=CARTESIAN_POINT('Ctrl Pts',(23.,33.3333333333333,-39.8371685740842));
#16247=CARTESIAN_POINT('Ctrl Pts',(33.6743371481683,33.125,-33.6743371481684));
#16248=CARTESIAN_POINT('Ctrl Pts',(39.8371685740842,32.9166666666667,-23.));
#16249=CARTESIAN_POINT('Ctrl Pts',(46.,32.7083333333333,-12.3256628518317));
#16250=CARTESIAN_POINT('Ctrl Pts',(46.,32.5,-5.63337527607782E-15));
#16251=CARTESIAN_POINT('Ctrl Pts',(46.,32.2916666666667,12.3256628518316));
#16252=CARTESIAN_POINT('Ctrl Pts',(39.8371685740842,32.0833333333333,23.));
#16253=CARTESIAN_POINT('Ctrl Pts',(33.6743371481684,31.875,33.6743371481683));
#16254=CARTESIAN_POINT('Ctrl Pts',(23.,31.6666666666667,39.8371685740842));
#16255=CARTESIAN_POINT('Ctrl Pts',(12.3256628518317,31.4583333333333,46.));
#16256=CARTESIAN_POINT('Ctrl Pts',(8.45006291411674E-15,31.25,46.));
#16257=CARTESIAN_POINT('Ctrl Pts',(-12.3256628518316,31.0416666666667,46.));
#16258=CARTESIAN_POINT('Ctrl Pts',(-23.,30.8333333333333,39.8371685740842));
#16259=CARTESIAN_POINT('Ctrl Pts',(-33.6743371481683,30.625,33.6743371481684));
#16260=CARTESIAN_POINT('Ctrl Pts',(-39.8371685740842,30.4166666666667,23.));
#16261=CARTESIAN_POINT('Ctrl Pts',(-46.,30.2083333333333,12.3256628518317));
#16262=CARTESIAN_POINT('Ctrl Pts',(-46.,30.,0.));
#16263=CARTESIAN_POINT('Ctrl Pts',(-45.858362923034,40.061608680256,3.60701400320328));
#16264=CARTESIAN_POINT('Ctrl Pts',(-46.089925771934,39.9280150456296,3.60701400320328));
#16265=CARTESIAN_POINT('Ctrl Pts',(-46.5530501979845,39.6608255719955,3.60701400320308));
#16266=CARTESIAN_POINT('Ctrl Pts',(-47.0161721905706,39.3936318804496,3.60701400320335));
#16267=CARTESIAN_POINT('Ctrl Pts',(-47.6893519862319,39.0052434879083,3.60701400320335));
#16268=CARTESIAN_POINT('Ctrl Pts',(-48.1309692507094,38.7504492807381,3.60701400320327));
#16269=CARTESIAN_POINT('Ctrl Pts',(-48.5725845633798,38.4956516907297,3.60701400320327));
#16270=CARTESIAN_POINT('Origin',(-4.32456261881337,-7931.57954062375,-4524.0108739909));
#16271=CARTESIAN_POINT('Ctrl Pts',(-48.706329375,58.437500006828,-1.8898197019151E-14));
#16272=CARTESIAN_POINT('Ctrl Pts',(-48.706329375,58.2291666734946,-13.0508216223155));
#16273=CARTESIAN_POINT('Ctrl Pts',(-42.1809185638422,58.0208333401613,-24.3531646875));
#16274=CARTESIAN_POINT('Ctrl Pts',(-35.6555077526845,57.812500006828,-35.6555077526845));
#16275=CARTESIAN_POINT('Ctrl Pts',(-24.3531646875,57.6041666734946,-42.1809185638422));
#16276=CARTESIAN_POINT('Ctrl Pts',(-13.0508216223155,57.3958333401613,-48.706329375));
#16277=CARTESIAN_POINT('Ctrl Pts',(1.59157945007855E-14,57.187500006828,
-48.706329375));
#16278=CARTESIAN_POINT('Ctrl Pts',(13.0508216223155,56.9791666734946,-48.706329375));
#16279=CARTESIAN_POINT('Ctrl Pts',(24.3531646875,56.7708333401613,-42.1809185638422));
#16280=CARTESIAN_POINT('Ctrl Pts',(35.6555077526845,56.562500006828,-35.6555077526845));
#16281=CARTESIAN_POINT('Ctrl Pts',(42.1809185638422,56.3541666734946,-24.3531646875));
#16282=CARTESIAN_POINT('Ctrl Pts',(48.706329375,56.1458333401613,-13.0508216223155));
#16283=CARTESIAN_POINT('Ctrl Pts',(48.706329375,55.937500006828,1.293339198242E-14));
#16284=CARTESIAN_POINT('Ctrl Pts',(48.706329375,55.7291666734946,13.0508216223155));
#16285=CARTESIAN_POINT('Ctrl Pts',(42.1809185638422,55.5208333401613,24.3531646875));
#16286=CARTESIAN_POINT('Ctrl Pts',(35.6555077526845,55.312500006828,35.6555077526845));
#16287=CARTESIAN_POINT('Ctrl Pts',(24.3531646875,55.1041666734946,42.1809185638422));
#16288=CARTESIAN_POINT('Ctrl Pts',(13.0508216223155,54.8958333401613,48.706329375));
#16289=CARTESIAN_POINT('Ctrl Pts',(-9.95098946405443E-15,54.687500006828,
48.706329375));
#16290=CARTESIAN_POINT('Ctrl Pts',(-13.0508216223155,54.4791666734946,48.706329375));
#16291=CARTESIAN_POINT('Ctrl Pts',(-24.3531646875,54.2708333401613,42.1809185638423));
#16292=CARTESIAN_POINT('Ctrl Pts',(-35.6555077526845,54.062500006828,35.6555077526845));
#16293=CARTESIAN_POINT('Ctrl Pts',(-42.1809185638422,53.8541666734946,24.3531646875));
#16294=CARTESIAN_POINT('Ctrl Pts',(-48.706329375,53.6458333401613,13.0508216223155));
#16295=CARTESIAN_POINT('Ctrl Pts',(-48.706329375,53.437500006828,-1.8898197019151E-14));
#16296=CARTESIAN_POINT('Ctrl Pts',(-48.706329375,53.2291666734946,-13.0508216223155));
#16297=CARTESIAN_POINT('Ctrl Pts',(-42.1809185638422,53.0208333401613,-24.3531646875));
#16298=CARTESIAN_POINT('Ctrl Pts',(-35.6555077526845,52.812500006828,-35.6555077526845));
#16299=CARTESIAN_POINT('Ctrl Pts',(-24.3531646875,52.6041666734946,-42.1809185638422));
#16300=CARTESIAN_POINT('Ctrl Pts',(-13.0508216223155,52.3958333401613,-48.706329375));
#16301=CARTESIAN_POINT('Ctrl Pts',(1.59157945007855E-14,52.187500006828,
-48.706329375));
#16302=CARTESIAN_POINT('Ctrl Pts',(13.0508216223155,51.9791666734946,-48.706329375));
#16303=CARTESIAN_POINT('Ctrl Pts',(24.3531646875,51.7708333401613,-42.1809185638422));
#16304=CARTESIAN_POINT('Ctrl Pts',(35.6555077526845,51.562500006828,-35.6555077526845));
#16305=CARTESIAN_POINT('Ctrl Pts',(42.1809185638422,51.3541666734946,-24.3531646875));
#16306=CARTESIAN_POINT('Ctrl Pts',(48.706329375,51.1458333401613,-13.0508216223155));
#16307=CARTESIAN_POINT('Ctrl Pts',(48.706329375,50.937500006828,1.293339198242E-14));
#16308=CARTESIAN_POINT('Ctrl Pts',(48.706329375,50.7291666734946,13.0508216223155));
#16309=CARTESIAN_POINT('Ctrl Pts',(42.1809185638422,50.5208333401613,24.3531646875));
#16310=CARTESIAN_POINT('Ctrl Pts',(35.6555077526845,50.312500006828,35.6555077526845));
#16311=CARTESIAN_POINT('Ctrl Pts',(24.3531646875,50.1041666734946,42.1809185638422));
#16312=CARTESIAN_POINT('Ctrl Pts',(13.0508216223155,49.8958333401613,48.706329375));
#16313=CARTESIAN_POINT('Ctrl Pts',(-9.95098946405443E-15,49.687500006828,
48.706329375));
#16314=CARTESIAN_POINT('Ctrl Pts',(-13.0508216223155,49.4791666734946,48.706329375));
#16315=CARTESIAN_POINT('Ctrl Pts',(-24.3531646875,49.2708333401613,42.1809185638423));
#16316=CARTESIAN_POINT('Ctrl Pts',(-35.6555077526845,49.062500006828,35.6555077526845));
#16317=CARTESIAN_POINT('Ctrl Pts',(-42.1809185638422,48.8541666734946,24.3531646875));
#16318=CARTESIAN_POINT('Ctrl Pts',(-48.706329375,48.6458333401613,13.0508216223155));
#16319=CARTESIAN_POINT('Ctrl Pts',(-48.706329375,48.437500006828,-1.8898197019151E-14));
#16320=CARTESIAN_POINT('Ctrl Pts',(-48.706329375,48.2291666734946,-13.0508216223155));
#16321=CARTESIAN_POINT('Ctrl Pts',(-42.1809185638422,48.0208333401613,-24.3531646875));
#16322=CARTESIAN_POINT('Ctrl Pts',(-35.6555077526845,47.812500006828,-35.6555077526845));
#16323=CARTESIAN_POINT('Ctrl Pts',(-24.3531646875,47.6041666734946,-42.1809185638422));
#16324=CARTESIAN_POINT('Ctrl Pts',(-13.0508216223155,47.3958333401613,-48.706329375));
#16325=CARTESIAN_POINT('Ctrl Pts',(1.59157945007855E-14,47.187500006828,
-48.706329375));
#16326=CARTESIAN_POINT('Ctrl Pts',(13.0508216223155,46.9791666734946,-48.706329375));
#16327=CARTESIAN_POINT('Ctrl Pts',(24.3531646875,46.7708333401613,-42.1809185638422));
#16328=CARTESIAN_POINT('Ctrl Pts',(35.6555077526845,46.562500006828,-35.6555077526845));
#16329=CARTESIAN_POINT('Ctrl Pts',(42.1809185638422,46.3541666734946,-24.3531646875));
#16330=CARTESIAN_POINT('Ctrl Pts',(48.706329375,46.1458333401613,-13.0508216223155));
#16331=CARTESIAN_POINT('Ctrl Pts',(48.706329375,45.937500006828,1.293339198242E-14));
#16332=CARTESIAN_POINT('Ctrl Pts',(48.706329375,45.7291666734946,13.0508216223155));
#16333=CARTESIAN_POINT('Ctrl Pts',(42.1809185638422,45.5208333401613,24.3531646875));
#16334=CARTESIAN_POINT('Ctrl Pts',(35.6555077526845,45.312500006828,35.6555077526845));
#16335=CARTESIAN_POINT('Ctrl Pts',(24.3531646875,45.1041666734946,42.1809185638422));
#16336=CARTESIAN_POINT('Ctrl Pts',(13.0508216223155,44.8958333401613,48.706329375));
#16337=CARTESIAN_POINT('Ctrl Pts',(-9.95098946405443E-15,44.687500006828,
48.706329375));
#16338=CARTESIAN_POINT('Ctrl Pts',(-13.0508216223155,44.4791666734946,48.706329375));
#16339=CARTESIAN_POINT('Ctrl Pts',(-24.3531646875,44.2708333401613,42.1809185638423));
#16340=CARTESIAN_POINT('Ctrl Pts',(-35.6555077526845,44.062500006828,35.6555077526845));
#16341=CARTESIAN_POINT('Ctrl Pts',(-42.1809185638422,43.8541666734946,24.3531646875));
#16342=CARTESIAN_POINT('Ctrl Pts',(-48.706329375,43.6458333401613,13.0508216223155));
#16343=CARTESIAN_POINT('Ctrl Pts',(-48.706329375,43.437500006828,-1.8898197019151E-14));
#16344=CARTESIAN_POINT('Ctrl Pts',(-48.706329375,43.2291666734946,-13.0508216223155));
#16345=CARTESIAN_POINT('Ctrl Pts',(-42.1809185638422,43.0208333401613,-24.3531646875));
#16346=CARTESIAN_POINT('Ctrl Pts',(-35.6555077526845,42.812500006828,-35.6555077526845));
#16347=CARTESIAN_POINT('Ctrl Pts',(-24.3531646875,42.6041666734946,-42.1809185638422));
#16348=CARTESIAN_POINT('Ctrl Pts',(-13.0508216223155,42.3958333401613,-48.706329375));
#16349=CARTESIAN_POINT('Ctrl Pts',(1.59157945007855E-14,42.187500006828,
-48.706329375));
#16350=CARTESIAN_POINT('Ctrl Pts',(13.0508216223155,41.9791666734946,-48.706329375));
#16351=CARTESIAN_POINT('Ctrl Pts',(24.3531646875,41.7708333401613,-42.1809185638422));
#16352=CARTESIAN_POINT('Ctrl Pts',(35.6555077526845,41.562500006828,-35.6555077526845));
#16353=CARTESIAN_POINT('Ctrl Pts',(42.1809185638422,41.3541666734946,-24.3531646875));
#16354=CARTESIAN_POINT('Ctrl Pts',(48.706329375,41.1458333401613,-13.0508216223155));
#16355=CARTESIAN_POINT('Ctrl Pts',(48.706329375,40.937500006828,1.293339198242E-14));
#16356=CARTESIAN_POINT('Ctrl Pts',(48.706329375,40.7291666734946,13.0508216223155));
#16357=CARTESIAN_POINT('Ctrl Pts',(42.1809185638422,40.5208333401613,24.3531646875));
#16358=CARTESIAN_POINT('Ctrl Pts',(35.6555077526845,40.312500006828,35.6555077526845));
#16359=CARTESIAN_POINT('Ctrl Pts',(24.3531646875,40.1041666734946,42.1809185638422));
#16360=CARTESIAN_POINT('Ctrl Pts',(13.0508216223155,39.8958333401613,48.706329375));
#16361=CARTESIAN_POINT('Ctrl Pts',(-9.95098946405443E-15,39.687500006828,
48.706329375));
#16362=CARTESIAN_POINT('Ctrl Pts',(-13.0508216223155,39.4791666734946,48.706329375));
#16363=CARTESIAN_POINT('Ctrl Pts',(-24.3531646875,39.2708333401613,42.1809185638423));
#16364=CARTESIAN_POINT('Ctrl Pts',(-35.6555077526845,39.062500006828,35.6555077526845));
#16365=CARTESIAN_POINT('Ctrl Pts',(-42.1809185638422,38.8541666734946,24.3531646875));
#16366=CARTESIAN_POINT('Ctrl Pts',(-48.706329375,38.6458333401613,13.0508216223155));
#16367=CARTESIAN_POINT('Ctrl Pts',(-48.706329375,38.437500006828,-1.8898197019151E-14));
#16368=CARTESIAN_POINT('Ctrl Pts',(-48.706329375,38.2291666734946,-13.0508216223155));
#16369=CARTESIAN_POINT('Ctrl Pts',(-42.1809185638422,38.0208333401613,-24.3531646875));
#16370=CARTESIAN_POINT('Ctrl Pts',(-35.6555077526845,37.812500006828,-35.6555077526845));
#16371=CARTESIAN_POINT('Ctrl Pts',(-24.3531646875,37.6041666734946,-42.1809185638422));
#16372=CARTESIAN_POINT('Ctrl Pts',(-13.0508216223155,37.3958333401613,-48.706329375));
#16373=CARTESIAN_POINT('Ctrl Pts',(1.59157945007855E-14,37.187500006828,
-48.706329375));
#16374=CARTESIAN_POINT('Ctrl Pts',(13.0508216223155,36.9791666734946,-48.706329375));
#16375=CARTESIAN_POINT('Ctrl Pts',(24.3531646875,36.7708333401613,-42.1809185638422));
#16376=CARTESIAN_POINT('Ctrl Pts',(35.6555077526845,36.562500006828,-35.6555077526845));
#16377=CARTESIAN_POINT('Ctrl Pts',(42.1809185638422,36.3541666734946,-24.3531646875));
#16378=CARTESIAN_POINT('Ctrl Pts',(48.706329375,36.1458333401613,-13.0508216223155));
#16379=CARTESIAN_POINT('Ctrl Pts',(48.706329375,35.937500006828,1.293339198242E-14));
#16380=CARTESIAN_POINT('Ctrl Pts',(48.706329375,35.7291666734946,13.0508216223155));
#16381=CARTESIAN_POINT('Ctrl Pts',(42.1809185638422,35.5208333401613,24.3531646875));
#16382=CARTESIAN_POINT('Ctrl Pts',(35.6555077526845,35.312500006828,35.6555077526845));
#16383=CARTESIAN_POINT('Ctrl Pts',(24.3531646875,35.1041666734946,42.1809185638422));
#16384=CARTESIAN_POINT('Ctrl Pts',(13.0508216223155,34.8958333401613,48.706329375));
#16385=CARTESIAN_POINT('Ctrl Pts',(-9.95098946405443E-15,34.687500006828,
48.706329375));
#16386=CARTESIAN_POINT('Ctrl Pts',(-13.0508216223155,34.4791666734946,48.706329375));
#16387=CARTESIAN_POINT('Ctrl Pts',(-24.3531646875,34.2708333401613,42.1809185638423));
#16388=CARTESIAN_POINT('Ctrl Pts',(-35.6555077526845,34.062500006828,35.6555077526845));
#16389=CARTESIAN_POINT('Ctrl Pts',(-42.1809185638422,33.8541666734946,24.3531646875));
#16390=CARTESIAN_POINT('Ctrl Pts',(-48.706329375,33.6458333401613,13.0508216223155));
#16391=CARTESIAN_POINT('Ctrl Pts',(-48.706329375,33.437500006828,-1.8898197019151E-14));
#16392=CARTESIAN_POINT('Ctrl Pts',(-48.706329375,33.2291666734946,-13.0508216223155));
#16393=CARTESIAN_POINT('Ctrl Pts',(-42.1809185638422,33.0208333401613,-24.3531646875));
#16394=CARTESIAN_POINT('Ctrl Pts',(-35.6555077526845,32.812500006828,-35.6555077526845));
#16395=CARTESIAN_POINT('Ctrl Pts',(-24.3531646875,32.6041666734946,-42.1809185638422));
#16396=CARTESIAN_POINT('Ctrl Pts',(-13.0508216223155,32.3958333401613,-48.706329375));
#16397=CARTESIAN_POINT('Ctrl Pts',(1.59157945007855E-14,32.187500006828,
-48.706329375));
#16398=CARTESIAN_POINT('Ctrl Pts',(13.0508216223155,31.9791666734946,-48.706329375));
#16399=CARTESIAN_POINT('Ctrl Pts',(24.3531646875,31.7708333401613,-42.1809185638422));
#16400=CARTESIAN_POINT('Ctrl Pts',(35.6555077526845,31.562500006828,-35.6555077526845));
#16401=CARTESIAN_POINT('Ctrl Pts',(42.1809185638422,31.3541666734946,-24.3531646875));
#16402=CARTESIAN_POINT('Ctrl Pts',(48.706329375,31.1458333401613,-13.0508216223155));
#16403=CARTESIAN_POINT('Ctrl Pts',(48.706329375,30.937500006828,1.293339198242E-14));
#16404=CARTESIAN_POINT('Ctrl Pts',(48.706329375,30.7291666734946,13.0508216223155));
#16405=CARTESIAN_POINT('Ctrl Pts',(42.1809185638422,30.5208333401613,24.3531646875));
#16406=CARTESIAN_POINT('Ctrl Pts',(35.6555077526845,30.312500006828,35.6555077526845));
#16407=CARTESIAN_POINT('Ctrl Pts',(24.3531646875,30.1041666734946,42.1809185638422));
#16408=CARTESIAN_POINT('Ctrl Pts',(13.0508216223155,29.8958333401613,48.706329375));
#16409=CARTESIAN_POINT('Ctrl Pts',(-9.95098946405443E-15,29.687500006828,
48.706329375));
#16410=CARTESIAN_POINT('Ctrl Pts',(-13.0508216223155,29.4791666734946,48.706329375));
#16411=CARTESIAN_POINT('Ctrl Pts',(-24.3531646875,29.2708333401613,42.1809185638423));
#16412=CARTESIAN_POINT('Ctrl Pts',(-35.6555077526845,29.062500006828,35.6555077526845));
#16413=CARTESIAN_POINT('Ctrl Pts',(-42.1809185638422,28.8541666734946,24.3531646875));
#16414=CARTESIAN_POINT('Ctrl Pts',(-48.706329375,28.6458333401613,13.0508216223155));
#16415=CARTESIAN_POINT('Ctrl Pts',(-48.706329375,28.437500006828,-1.8898197019151E-14));
#16416=CARTESIAN_POINT('Ctrl Pts',(-46.,60.,0.));
#16417=CARTESIAN_POINT('Ctrl Pts',(-46.,59.7916666666667,-12.3256628518316));
#16418=CARTESIAN_POINT('Ctrl Pts',(-39.8371685740842,59.5833333333333,-23.));
#16419=CARTESIAN_POINT('Ctrl Pts',(-33.6743371481684,59.375,-33.6743371481684));
#16420=CARTESIAN_POINT('Ctrl Pts',(-23.,59.1666666666667,-39.8371685740842));
#16421=CARTESIAN_POINT('Ctrl Pts',(-12.3256628518317,58.9583333333333,-46.));
#16422=CARTESIAN_POINT('Ctrl Pts',(-2.81668763803891E-15,58.75,-46.));
#16423=CARTESIAN_POINT('Ctrl Pts',(12.3256628518316,58.5416666666667,-46.));
#16424=CARTESIAN_POINT('Ctrl Pts',(23.,58.3333333333333,-39.8371685740842));
#16425=CARTESIAN_POINT('Ctrl Pts',(33.6743371481683,58.125,-33.6743371481684));
#16426=CARTESIAN_POINT('Ctrl Pts',(39.8371685740842,57.9166666666667,-23.));
#16427=CARTESIAN_POINT('Ctrl Pts',(46.,57.7083333333333,-12.3256628518317));
#16428=CARTESIAN_POINT('Ctrl Pts',(46.,57.5,-5.63337527607782E-15));
#16429=CARTESIAN_POINT('Ctrl Pts',(46.,57.2916666666667,12.3256628518316));
#16430=CARTESIAN_POINT('Ctrl Pts',(39.8371685740842,57.0833333333333,23.));
#16431=CARTESIAN_POINT('Ctrl Pts',(33.6743371481684,56.875,33.6743371481683));
#16432=CARTESIAN_POINT('Ctrl Pts',(23.,56.6666666666667,39.8371685740842));
#16433=CARTESIAN_POINT('Ctrl Pts',(12.3256628518317,56.4583333333333,46.));
#16434=CARTESIAN_POINT('Ctrl Pts',(8.45006291411674E-15,56.25,46.));
#16435=CARTESIAN_POINT('Ctrl Pts',(-12.3256628518316,56.0416666666667,46.));
#16436=CARTESIAN_POINT('Ctrl Pts',(-23.,55.8333333333333,39.8371685740842));
#16437=CARTESIAN_POINT('Ctrl Pts',(-33.6743371481683,55.625,33.6743371481684));
#16438=CARTESIAN_POINT('Ctrl Pts',(-39.8371685740842,55.4166666666667,23.));
#16439=CARTESIAN_POINT('Ctrl Pts',(-46.,55.2083333333333,12.3256628518317));
#16440=CARTESIAN_POINT('Ctrl Pts',(-46.,55.,0.));
#16441=CARTESIAN_POINT('Ctrl Pts',(-46.,54.7916666666667,-12.3256628518316));
#16442=CARTESIAN_POINT('Ctrl Pts',(-39.8371685740842,54.5833333333333,-23.));
#16443=CARTESIAN_POINT('Ctrl Pts',(-33.6743371481684,54.375,-33.6743371481684));
#16444=CARTESIAN_POINT('Ctrl Pts',(-23.,54.1666666666667,-39.8371685740842));
#16445=CARTESIAN_POINT('Ctrl Pts',(-12.3256628518317,53.9583333333333,-46.));
#16446=CARTESIAN_POINT('Ctrl Pts',(-2.81668763803891E-15,53.75,-46.));
#16447=CARTESIAN_POINT('Ctrl Pts',(12.3256628518316,53.5416666666667,-46.));
#16448=CARTESIAN_POINT('Ctrl Pts',(23.,53.3333333333333,-39.8371685740842));
#16449=CARTESIAN_POINT('Ctrl Pts',(33.6743371481683,53.125,-33.6743371481684));
#16450=CARTESIAN_POINT('Ctrl Pts',(39.8371685740842,52.9166666666667,-23.));
#16451=CARTESIAN_POINT('Ctrl Pts',(46.,52.7083333333333,-12.3256628518317));
#16452=CARTESIAN_POINT('Ctrl Pts',(46.,52.5,-5.63337527607782E-15));
#16453=CARTESIAN_POINT('Ctrl Pts',(46.,52.2916666666667,12.3256628518316));
#16454=CARTESIAN_POINT('Ctrl Pts',(39.8371685740842,52.0833333333333,23.));
#16455=CARTESIAN_POINT('Ctrl Pts',(33.6743371481684,51.875,33.6743371481683));
#16456=CARTESIAN_POINT('Ctrl Pts',(23.,51.6666666666667,39.8371685740842));
#16457=CARTESIAN_POINT('Ctrl Pts',(12.3256628518317,51.4583333333333,46.));
#16458=CARTESIAN_POINT('Ctrl Pts',(8.45006291411674E-15,51.25,46.));
#16459=CARTESIAN_POINT('Ctrl Pts',(-12.3256628518316,51.0416666666667,46.));
#16460=CARTESIAN_POINT('Ctrl Pts',(-23.,50.8333333333333,39.8371685740842));
#16461=CARTESIAN_POINT('Ctrl Pts',(-33.6743371481683,50.625,33.6743371481684));
#16462=CARTESIAN_POINT('Ctrl Pts',(-39.8371685740842,50.4166666666667,23.));
#16463=CARTESIAN_POINT('Ctrl Pts',(-46.,50.2083333333333,12.3256628518317));
#16464=CARTESIAN_POINT('Ctrl Pts',(-46.,50.,0.));
#16465=CARTESIAN_POINT('Ctrl Pts',(-46.,49.7916666666667,-12.3256628518316));
#16466=CARTESIAN_POINT('Ctrl Pts',(-39.8371685740842,49.5833333333333,-23.));
#16467=CARTESIAN_POINT('Ctrl Pts',(-33.6743371481684,49.375,-33.6743371481684));
#16468=CARTESIAN_POINT('Ctrl Pts',(-23.,49.1666666666667,-39.8371685740842));
#16469=CARTESIAN_POINT('Ctrl Pts',(-12.3256628518317,48.9583333333333,-46.));
#16470=CARTESIAN_POINT('Ctrl Pts',(-2.81668763803891E-15,48.75,-46.));
#16471=CARTESIAN_POINT('Ctrl Pts',(12.3256628518316,48.5416666666667,-46.));
#16472=CARTESIAN_POINT('Ctrl Pts',(23.,48.3333333333333,-39.8371685740842));
#16473=CARTESIAN_POINT('Ctrl Pts',(33.6743371481683,48.125,-33.6743371481684));
#16474=CARTESIAN_POINT('Ctrl Pts',(39.8371685740842,47.9166666666667,-23.));
#16475=CARTESIAN_POINT('Ctrl Pts',(46.,47.7083333333333,-12.3256628518317));
#16476=CARTESIAN_POINT('Ctrl Pts',(46.,47.5,-5.63337527607782E-15));
#16477=CARTESIAN_POINT('Ctrl Pts',(46.,47.2916666666667,12.3256628518316));
#16478=CARTESIAN_POINT('Ctrl Pts',(39.8371685740842,47.0833333333333,23.));
#16479=CARTESIAN_POINT('Ctrl Pts',(33.6743371481684,46.875,33.6743371481683));
#16480=CARTESIAN_POINT('Ctrl Pts',(23.,46.6666666666667,39.8371685740842));
#16481=CARTESIAN_POINT('Ctrl Pts',(12.3256628518317,46.4583333333333,46.));
#16482=CARTESIAN_POINT('Ctrl Pts',(8.45006291411674E-15,46.25,46.));
#16483=CARTESIAN_POINT('Ctrl Pts',(-12.3256628518316,46.0416666666667,46.));
#16484=CARTESIAN_POINT('Ctrl Pts',(-23.,45.8333333333333,39.8371685740842));
#16485=CARTESIAN_POINT('Ctrl Pts',(-33.6743371481683,45.625,33.6743371481684));
#16486=CARTESIAN_POINT('Ctrl Pts',(-39.8371685740842,45.4166666666667,23.));
#16487=CARTESIAN_POINT('Ctrl Pts',(-46.,45.2083333333333,12.3256628518317));
#16488=CARTESIAN_POINT('Ctrl Pts',(-46.,45.,0.));
#16489=CARTESIAN_POINT('Ctrl Pts',(-46.,44.7916666666667,-12.3256628518316));
#16490=CARTESIAN_POINT('Ctrl Pts',(-39.8371685740842,44.5833333333333,-23.));
#16491=CARTESIAN_POINT('Ctrl Pts',(-33.6743371481684,44.375,-33.6743371481684));
#16492=CARTESIAN_POINT('Ctrl Pts',(-23.,44.1666666666667,-39.8371685740842));
#16493=CARTESIAN_POINT('Ctrl Pts',(-12.3256628518317,43.9583333333333,-46.));
#16494=CARTESIAN_POINT('Ctrl Pts',(-2.81668763803891E-15,43.75,-46.));
#16495=CARTESIAN_POINT('Ctrl Pts',(12.3256628518316,43.5416666666667,-46.));
#16496=CARTESIAN_POINT('Ctrl Pts',(23.,43.3333333333333,-39.8371685740842));
#16497=CARTESIAN_POINT('Ctrl Pts',(33.6743371481683,43.125,-33.6743371481684));
#16498=CARTESIAN_POINT('Ctrl Pts',(39.8371685740842,42.9166666666667,-23.));
#16499=CARTESIAN_POINT('Ctrl Pts',(46.,42.7083333333333,-12.3256628518317));
#16500=CARTESIAN_POINT('Ctrl Pts',(46.,42.5,-5.63337527607782E-15));
#16501=CARTESIAN_POINT('Ctrl Pts',(46.,42.2916666666667,12.3256628518316));
#16502=CARTESIAN_POINT('Ctrl Pts',(39.8371685740842,42.0833333333333,23.));
#16503=CARTESIAN_POINT('Ctrl Pts',(33.6743371481684,41.875,33.6743371481683));
#16504=CARTESIAN_POINT('Ctrl Pts',(23.,41.6666666666667,39.8371685740842));
#16505=CARTESIAN_POINT('Ctrl Pts',(12.3256628518317,41.4583333333333,46.));
#16506=CARTESIAN_POINT('Ctrl Pts',(8.45006291411674E-15,41.25,46.));
#16507=CARTESIAN_POINT('Ctrl Pts',(-12.3256628518316,41.0416666666667,46.));
#16508=CARTESIAN_POINT('Ctrl Pts',(-23.,40.8333333333333,39.8371685740842));
#16509=CARTESIAN_POINT('Ctrl Pts',(-33.6743371481683,40.625,33.6743371481684));
#16510=CARTESIAN_POINT('Ctrl Pts',(-39.8371685740842,40.4166666666667,23.));
#16511=CARTESIAN_POINT('Ctrl Pts',(-46.,40.2083333333333,12.3256628518317));
#16512=CARTESIAN_POINT('Ctrl Pts',(-46.,40.,0.));
#16513=CARTESIAN_POINT('Ctrl Pts',(-46.,39.7916666666667,-12.3256628518316));
#16514=CARTESIAN_POINT('Ctrl Pts',(-39.8371685740842,39.5833333333333,-23.));
#16515=CARTESIAN_POINT('Ctrl Pts',(-33.6743371481684,39.375,-33.6743371481684));
#16516=CARTESIAN_POINT('Ctrl Pts',(-23.,39.1666666666667,-39.8371685740842));
#16517=CARTESIAN_POINT('Ctrl Pts',(-12.3256628518317,38.9583333333333,-46.));
#16518=CARTESIAN_POINT('Ctrl Pts',(-2.81668763803891E-15,38.75,-46.));
#16519=CARTESIAN_POINT('Ctrl Pts',(12.3256628518316,38.5416666666667,-46.));
#16520=CARTESIAN_POINT('Ctrl Pts',(23.,38.3333333333333,-39.8371685740842));
#16521=CARTESIAN_POINT('Ctrl Pts',(33.6743371481683,38.125,-33.6743371481684));
#16522=CARTESIAN_POINT('Ctrl Pts',(39.8371685740842,37.9166666666667,-23.));
#16523=CARTESIAN_POINT('Ctrl Pts',(46.,37.7083333333333,-12.3256628518317));
#16524=CARTESIAN_POINT('Ctrl Pts',(46.,37.5,-5.63337527607782E-15));
#16525=CARTESIAN_POINT('Ctrl Pts',(46.,37.2916666666667,12.3256628518316));
#16526=CARTESIAN_POINT('Ctrl Pts',(39.8371685740842,37.0833333333333,23.));
#16527=CARTESIAN_POINT('Ctrl Pts',(33.6743371481684,36.875,33.6743371481683));
#16528=CARTESIAN_POINT('Ctrl Pts',(23.,36.6666666666667,39.8371685740842));
#16529=CARTESIAN_POINT('Ctrl Pts',(12.3256628518317,36.4583333333333,46.));
#16530=CARTESIAN_POINT('Ctrl Pts',(8.45006291411674E-15,36.25,46.));
#16531=CARTESIAN_POINT('Ctrl Pts',(-12.3256628518316,36.0416666666667,46.));
#16532=CARTESIAN_POINT('Ctrl Pts',(-23.,35.8333333333333,39.8371685740842));
#16533=CARTESIAN_POINT('Ctrl Pts',(-33.6743371481683,35.625,33.6743371481684));
#16534=CARTESIAN_POINT('Ctrl Pts',(-39.8371685740842,35.4166666666667,23.));
#16535=CARTESIAN_POINT('Ctrl Pts',(-46.,35.2083333333333,12.3256628518317));
#16536=CARTESIAN_POINT('Ctrl Pts',(-46.,35.,0.));
#16537=CARTESIAN_POINT('Ctrl Pts',(-46.,34.7916666666667,-12.3256628518316));
#16538=CARTESIAN_POINT('Ctrl Pts',(-39.8371685740842,34.5833333333333,-23.));
#16539=CARTESIAN_POINT('Ctrl Pts',(-33.6743371481684,34.375,-33.6743371481684));
#16540=CARTESIAN_POINT('Ctrl Pts',(-23.,34.1666666666667,-39.8371685740842));
#16541=CARTESIAN_POINT('Ctrl Pts',(-12.3256628518317,33.9583333333333,-46.));
#16542=CARTESIAN_POINT('Ctrl Pts',(-2.81668763803891E-15,33.75,-46.));
#16543=CARTESIAN_POINT('Ctrl Pts',(12.3256628518316,33.5416666666667,-46.));
#16544=CARTESIAN_POINT('Ctrl Pts',(23.,33.3333333333333,-39.8371685740842));
#16545=CARTESIAN_POINT('Ctrl Pts',(33.6743371481683,33.125,-33.6743371481684));
#16546=CARTESIAN_POINT('Ctrl Pts',(39.8371685740842,32.9166666666667,-23.));
#16547=CARTESIAN_POINT('Ctrl Pts',(46.,32.7083333333333,-12.3256628518317));
#16548=CARTESIAN_POINT('Ctrl Pts',(46.,32.5,-5.63337527607782E-15));
#16549=CARTESIAN_POINT('Ctrl Pts',(46.,32.2916666666667,12.3256628518316));
#16550=CARTESIAN_POINT('Ctrl Pts',(39.8371685740842,32.0833333333333,23.));
#16551=CARTESIAN_POINT('Ctrl Pts',(33.6743371481684,31.875,33.6743371481683));
#16552=CARTESIAN_POINT('Ctrl Pts',(23.,31.6666666666667,39.8371685740842));
#16553=CARTESIAN_POINT('Ctrl Pts',(12.3256628518317,31.4583333333333,46.));
#16554=CARTESIAN_POINT('Ctrl Pts',(8.45006291411674E-15,31.25,46.));
#16555=CARTESIAN_POINT('Ctrl Pts',(-12.3256628518316,31.0416666666667,46.));
#16556=CARTESIAN_POINT('Ctrl Pts',(-23.,30.8333333333333,39.8371685740842));
#16557=CARTESIAN_POINT('Ctrl Pts',(-33.6743371481683,30.625,33.6743371481684));
#16558=CARTESIAN_POINT('Ctrl Pts',(-39.8371685740842,30.4166666666667,23.));
#16559=CARTESIAN_POINT('Ctrl Pts',(-46.,30.2083333333333,12.3256628518317));
#16560=CARTESIAN_POINT('Ctrl Pts',(-46.,30.,0.));
#16561=CARTESIAN_POINT('Ctrl Pts',(45.7957082162897,37.5741208584476,-4.33048599679664));
#16562=CARTESIAN_POINT('Ctrl Pts',(46.027322302781,37.4406160752063,-4.33048599679664));
#16563=CARTESIAN_POINT('Ctrl Pts',(46.4905476657728,37.1736016336912,-4.33048599679679));
#16564=CARTESIAN_POINT('Ctrl Pts',(46.9537676533565,36.9065778670208,-4.33048599679665));
#16565=CARTESIAN_POINT('Ctrl Pts',(47.6280672732221,36.5178683162597,-4.33048599679665));
#16566=CARTESIAN_POINT('Ctrl Pts',(48.0707534890442,36.2626647328764,-4.33048599679682));
#16567=CARTESIAN_POINT('Ctrl Pts',(48.5134353784344,36.0074536451604,-4.33048599679682));
#16568=CARTESIAN_POINT('Ctrl Pts',(3.61292728433801,37.1292520480092,-48.5721450795008));
#16569=CARTESIAN_POINT('Ctrl Pts',(3.61292728433801,37.2624339185675,-48.3403451622817));
#16570=CARTESIAN_POINT('Ctrl Pts',(3.61292728433802,37.395608829009,-48.1085412459393));
#16571=CARTESIAN_POINT('Ctrl Pts',(3.61292728433802,37.6619441142016,-47.6449250631479));
#16572=CARTESIAN_POINT('Ctrl Pts',(3.61292728433795,37.7951044891727,-47.4131127965212));
#16573=CARTESIAN_POINT('Ctrl Pts',(3.61292728433795,37.9282572703914,-47.1812961682826));
#16574=CARTESIAN_POINT('Ctrl Pts',(3.61292728433795,38.1816295626638,-46.7401795055578));
#16575=CARTESIAN_POINT('Ctrl Pts',(3.61292728433797,38.4349743764897,-46.2990470581854));
#16576=CARTESIAN_POINT('Ctrl Pts',(3.61292728433797,38.688289262853,-45.8578974271399));
#16577=CARTESIAN_POINT('Ctrl Pts',(-48.706329375,58.437500006828,-1.8898197019151E-14));
#16578=CARTESIAN_POINT('Ctrl Pts',(-48.706329375,58.2291666734946,-13.0508216223155));
#16579=CARTESIAN_POINT('Ctrl Pts',(-42.1809185638422,58.0208333401613,-24.3531646875));
#16580=CARTESIAN_POINT('Ctrl Pts',(-35.6555077526845,57.812500006828,-35.6555077526845));
#16581=CARTESIAN_POINT('Ctrl Pts',(-24.3531646875,57.6041666734946,-42.1809185638422));
#16582=CARTESIAN_POINT('Ctrl Pts',(-13.0508216223155,57.3958333401613,-48.706329375));
#16583=CARTESIAN_POINT('Ctrl Pts',(1.59157945007855E-14,57.187500006828,
-48.706329375));
#16584=CARTESIAN_POINT('Ctrl Pts',(13.0508216223155,56.9791666734946,-48.706329375));
#16585=CARTESIAN_POINT('Ctrl Pts',(24.3531646875,56.7708333401613,-42.1809185638422));
#16586=CARTESIAN_POINT('Ctrl Pts',(35.6555077526845,56.562500006828,-35.6555077526845));
#16587=CARTESIAN_POINT('Ctrl Pts',(42.1809185638422,56.3541666734946,-24.3531646875));
#16588=CARTESIAN_POINT('Ctrl Pts',(48.706329375,56.1458333401613,-13.0508216223155));
#16589=CARTESIAN_POINT('Ctrl Pts',(48.706329375,55.937500006828,1.293339198242E-14));
#16590=CARTESIAN_POINT('Ctrl Pts',(48.706329375,55.7291666734946,13.0508216223155));
#16591=CARTESIAN_POINT('Ctrl Pts',(42.1809185638422,55.5208333401613,24.3531646875));
#16592=CARTESIAN_POINT('Ctrl Pts',(35.6555077526845,55.312500006828,35.6555077526845));
#16593=CARTESIAN_POINT('Ctrl Pts',(24.3531646875,55.1041666734946,42.1809185638422));
#16594=CARTESIAN_POINT('Ctrl Pts',(13.0508216223155,54.8958333401613,48.706329375));
#16595=CARTESIAN_POINT('Ctrl Pts',(-9.95098946405443E-15,54.687500006828,
48.706329375));
#16596=CARTESIAN_POINT('Ctrl Pts',(-13.0508216223155,54.4791666734946,48.706329375));
#16597=CARTESIAN_POINT('Ctrl Pts',(-24.3531646875,54.2708333401613,42.1809185638423));
#16598=CARTESIAN_POINT('Ctrl Pts',(-35.6555077526845,54.062500006828,35.6555077526845));
#16599=CARTESIAN_POINT('Ctrl Pts',(-42.1809185638422,53.8541666734946,24.3531646875));
#16600=CARTESIAN_POINT('Ctrl Pts',(-48.706329375,53.6458333401613,13.0508216223155));
#16601=CARTESIAN_POINT('Ctrl Pts',(-48.706329375,53.437500006828,-1.8898197019151E-14));
#16602=CARTESIAN_POINT('Ctrl Pts',(-48.706329375,53.2291666734946,-13.0508216223155));
#16603=CARTESIAN_POINT('Ctrl Pts',(-42.1809185638422,53.0208333401613,-24.3531646875));
#16604=CARTESIAN_POINT('Ctrl Pts',(-35.6555077526845,52.812500006828,-35.6555077526845));
#16605=CARTESIAN_POINT('Ctrl Pts',(-24.3531646875,52.6041666734946,-42.1809185638422));
#16606=CARTESIAN_POINT('Ctrl Pts',(-13.0508216223155,52.3958333401613,-48.706329375));
#16607=CARTESIAN_POINT('Ctrl Pts',(1.59157945007855E-14,52.187500006828,
-48.706329375));
#16608=CARTESIAN_POINT('Ctrl Pts',(13.0508216223155,51.9791666734946,-48.706329375));
#16609=CARTESIAN_POINT('Ctrl Pts',(24.3531646875,51.7708333401613,-42.1809185638422));
#16610=CARTESIAN_POINT('Ctrl Pts',(35.6555077526845,51.562500006828,-35.6555077526845));
#16611=CARTESIAN_POINT('Ctrl Pts',(42.1809185638422,51.3541666734946,-24.3531646875));
#16612=CARTESIAN_POINT('Ctrl Pts',(48.706329375,51.1458333401613,-13.0508216223155));
#16613=CARTESIAN_POINT('Ctrl Pts',(48.706329375,50.937500006828,1.293339198242E-14));
#16614=CARTESIAN_POINT('Ctrl Pts',(48.706329375,50.7291666734946,13.0508216223155));
#16615=CARTESIAN_POINT('Ctrl Pts',(42.1809185638422,50.5208333401613,24.3531646875));
#16616=CARTESIAN_POINT('Ctrl Pts',(35.6555077526845,50.312500006828,35.6555077526845));
#16617=CARTESIAN_POINT('Ctrl Pts',(24.3531646875,50.1041666734946,42.1809185638422));
#16618=CARTESIAN_POINT('Ctrl Pts',(13.0508216223155,49.8958333401613,48.706329375));
#16619=CARTESIAN_POINT('Ctrl Pts',(-9.95098946405443E-15,49.687500006828,
48.706329375));
#16620=CARTESIAN_POINT('Ctrl Pts',(-13.0508216223155,49.4791666734946,48.706329375));
#16621=CARTESIAN_POINT('Ctrl Pts',(-24.3531646875,49.2708333401613,42.1809185638423));
#16622=CARTESIAN_POINT('Ctrl Pts',(-35.6555077526845,49.062500006828,35.6555077526845));
#16623=CARTESIAN_POINT('Ctrl Pts',(-42.1809185638422,48.8541666734946,24.3531646875));
#16624=CARTESIAN_POINT('Ctrl Pts',(-48.706329375,48.6458333401613,13.0508216223155));
#16625=CARTESIAN_POINT('Ctrl Pts',(-48.706329375,48.437500006828,-1.8898197019151E-14));
#16626=CARTESIAN_POINT('Ctrl Pts',(-48.706329375,48.2291666734946,-13.0508216223155));
#16627=CARTESIAN_POINT('Ctrl Pts',(-42.1809185638422,48.0208333401613,-24.3531646875));
#16628=CARTESIAN_POINT('Ctrl Pts',(-35.6555077526845,47.812500006828,-35.6555077526845));
#16629=CARTESIAN_POINT('Ctrl Pts',(-24.3531646875,47.6041666734946,-42.1809185638422));
#16630=CARTESIAN_POINT('Ctrl Pts',(-13.0508216223155,47.3958333401613,-48.706329375));
#16631=CARTESIAN_POINT('Ctrl Pts',(1.59157945007855E-14,47.187500006828,
-48.706329375));
#16632=CARTESIAN_POINT('Ctrl Pts',(13.0508216223155,46.9791666734946,-48.706329375));
#16633=CARTESIAN_POINT('Ctrl Pts',(24.3531646875,46.7708333401613,-42.1809185638422));
#16634=CARTESIAN_POINT('Ctrl Pts',(35.6555077526845,46.562500006828,-35.6555077526845));
#16635=CARTESIAN_POINT('Ctrl Pts',(42.1809185638422,46.3541666734946,-24.3531646875));
#16636=CARTESIAN_POINT('Ctrl Pts',(48.706329375,46.1458333401613,-13.0508216223155));
#16637=CARTESIAN_POINT('Ctrl Pts',(48.706329375,45.937500006828,1.293339198242E-14));
#16638=CARTESIAN_POINT('Ctrl Pts',(48.706329375,45.7291666734946,13.0508216223155));
#16639=CARTESIAN_POINT('Ctrl Pts',(42.1809185638422,45.5208333401613,24.3531646875));
#16640=CARTESIAN_POINT('Ctrl Pts',(35.6555077526845,45.312500006828,35.6555077526845));
#16641=CARTESIAN_POINT('Ctrl Pts',(24.3531646875,45.1041666734946,42.1809185638422));
#16642=CARTESIAN_POINT('Ctrl Pts',(13.0508216223155,44.8958333401613,48.706329375));
#16643=CARTESIAN_POINT('Ctrl Pts',(-9.95098946405443E-15,44.687500006828,
48.706329375));
#16644=CARTESIAN_POINT('Ctrl Pts',(-13.0508216223155,44.4791666734946,48.706329375));
#16645=CARTESIAN_POINT('Ctrl Pts',(-24.3531646875,44.2708333401613,42.1809185638423));
#16646=CARTESIAN_POINT('Ctrl Pts',(-35.6555077526845,44.062500006828,35.6555077526845));
#16647=CARTESIAN_POINT('Ctrl Pts',(-42.1809185638422,43.8541666734946,24.3531646875));
#16648=CARTESIAN_POINT('Ctrl Pts',(-48.706329375,43.6458333401613,13.0508216223155));
#16649=CARTESIAN_POINT('Ctrl Pts',(-48.706329375,43.437500006828,-1.8898197019151E-14));
#16650=CARTESIAN_POINT('Ctrl Pts',(-48.706329375,43.2291666734946,-13.0508216223155));
#16651=CARTESIAN_POINT('Ctrl Pts',(-42.1809185638422,43.0208333401613,-24.3531646875));
#16652=CARTESIAN_POINT('Ctrl Pts',(-35.6555077526845,42.812500006828,-35.6555077526845));
#16653=CARTESIAN_POINT('Ctrl Pts',(-24.3531646875,42.6041666734946,-42.1809185638422));
#16654=CARTESIAN_POINT('Ctrl Pts',(-13.0508216223155,42.3958333401613,-48.706329375));
#16655=CARTESIAN_POINT('Ctrl Pts',(1.59157945007855E-14,42.187500006828,
-48.706329375));
#16656=CARTESIAN_POINT('Ctrl Pts',(13.0508216223155,41.9791666734946,-48.706329375));
#16657=CARTESIAN_POINT('Ctrl Pts',(24.3531646875,41.7708333401613,-42.1809185638422));
#16658=CARTESIAN_POINT('Ctrl Pts',(35.6555077526845,41.562500006828,-35.6555077526845));
#16659=CARTESIAN_POINT('Ctrl Pts',(42.1809185638422,41.3541666734946,-24.3531646875));
#16660=CARTESIAN_POINT('Ctrl Pts',(48.706329375,41.1458333401613,-13.0508216223155));
#16661=CARTESIAN_POINT('Ctrl Pts',(48.706329375,40.937500006828,1.293339198242E-14));
#16662=CARTESIAN_POINT('Ctrl Pts',(48.706329375,40.7291666734946,13.0508216223155));
#16663=CARTESIAN_POINT('Ctrl Pts',(42.1809185638422,40.5208333401613,24.3531646875));
#16664=CARTESIAN_POINT('Ctrl Pts',(35.6555077526845,40.312500006828,35.6555077526845));
#16665=CARTESIAN_POINT('Ctrl Pts',(24.3531646875,40.1041666734946,42.1809185638422));
#16666=CARTESIAN_POINT('Ctrl Pts',(13.0508216223155,39.8958333401613,48.706329375));
#16667=CARTESIAN_POINT('Ctrl Pts',(-9.95098946405443E-15,39.687500006828,
48.706329375));
#16668=CARTESIAN_POINT('Ctrl Pts',(-13.0508216223155,39.4791666734946,48.706329375));
#16669=CARTESIAN_POINT('Ctrl Pts',(-24.3531646875,39.2708333401613,42.1809185638423));
#16670=CARTESIAN_POINT('Ctrl Pts',(-35.6555077526845,39.062500006828,35.6555077526845));
#16671=CARTESIAN_POINT('Ctrl Pts',(-42.1809185638422,38.8541666734946,24.3531646875));
#16672=CARTESIAN_POINT('Ctrl Pts',(-48.706329375,38.6458333401613,13.0508216223155));
#16673=CARTESIAN_POINT('Ctrl Pts',(-48.706329375,38.437500006828,-1.8898197019151E-14));
#16674=CARTESIAN_POINT('Ctrl Pts',(-48.706329375,38.2291666734946,-13.0508216223155));
#16675=CARTESIAN_POINT('Ctrl Pts',(-42.1809185638422,38.0208333401613,-24.3531646875));
#16676=CARTESIAN_POINT('Ctrl Pts',(-35.6555077526845,37.812500006828,-35.6555077526845));
#16677=CARTESIAN_POINT('Ctrl Pts',(-24.3531646875,37.6041666734946,-42.1809185638422));
#16678=CARTESIAN_POINT('Ctrl Pts',(-13.0508216223155,37.3958333401613,-48.706329375));
#16679=CARTESIAN_POINT('Ctrl Pts',(1.59157945007855E-14,37.187500006828,
-48.706329375));
#16680=CARTESIAN_POINT('Ctrl Pts',(13.0508216223155,36.9791666734946,-48.706329375));
#16681=CARTESIAN_POINT('Ctrl Pts',(24.3531646875,36.7708333401613,-42.1809185638422));
#16682=CARTESIAN_POINT('Ctrl Pts',(35.6555077526845,36.562500006828,-35.6555077526845));
#16683=CARTESIAN_POINT('Ctrl Pts',(42.1809185638422,36.3541666734946,-24.3531646875));
#16684=CARTESIAN_POINT('Ctrl Pts',(48.706329375,36.1458333401613,-13.0508216223155));
#16685=CARTESIAN_POINT('Ctrl Pts',(48.706329375,35.937500006828,1.293339198242E-14));
#16686=CARTESIAN_POINT('Ctrl Pts',(48.706329375,35.7291666734946,13.0508216223155));
#16687=CARTESIAN_POINT('Ctrl Pts',(42.1809185638422,35.5208333401613,24.3531646875));
#16688=CARTESIAN_POINT('Ctrl Pts',(35.6555077526845,35.312500006828,35.6555077526845));
#16689=CARTESIAN_POINT('Ctrl Pts',(24.3531646875,35.1041666734946,42.1809185638422));
#16690=CARTESIAN_POINT('Ctrl Pts',(13.0508216223155,34.8958333401613,48.706329375));
#16691=CARTESIAN_POINT('Ctrl Pts',(-9.95098946405443E-15,34.687500006828,
48.706329375));
#16692=CARTESIAN_POINT('Ctrl Pts',(-13.0508216223155,34.4791666734946,48.706329375));
#16693=CARTESIAN_POINT('Ctrl Pts',(-24.3531646875,34.2708333401613,42.1809185638423));
#16694=CARTESIAN_POINT('Ctrl Pts',(-35.6555077526845,34.062500006828,35.6555077526845));
#16695=CARTESIAN_POINT('Ctrl Pts',(-42.1809185638422,33.8541666734946,24.3531646875));
#16696=CARTESIAN_POINT('Ctrl Pts',(-48.706329375,33.6458333401613,13.0508216223155));
#16697=CARTESIAN_POINT('Ctrl Pts',(-48.706329375,33.437500006828,-1.8898197019151E-14));
#16698=CARTESIAN_POINT('Ctrl Pts',(-48.706329375,33.2291666734946,-13.0508216223155));
#16699=CARTESIAN_POINT('Ctrl Pts',(-42.1809185638422,33.0208333401613,-24.3531646875));
#16700=CARTESIAN_POINT('Ctrl Pts',(-35.6555077526845,32.812500006828,-35.6555077526845));
#16701=CARTESIAN_POINT('Ctrl Pts',(-24.3531646875,32.6041666734946,-42.1809185638422));
#16702=CARTESIAN_POINT('Ctrl Pts',(-13.0508216223155,32.3958333401613,-48.706329375));
#16703=CARTESIAN_POINT('Ctrl Pts',(1.59157945007855E-14,32.187500006828,
-48.706329375));
#16704=CARTESIAN_POINT('Ctrl Pts',(13.0508216223155,31.9791666734946,-48.706329375));
#16705=CARTESIAN_POINT('Ctrl Pts',(24.3531646875,31.7708333401613,-42.1809185638422));
#16706=CARTESIAN_POINT('Ctrl Pts',(35.6555077526845,31.562500006828,-35.6555077526845));
#16707=CARTESIAN_POINT('Ctrl Pts',(42.1809185638422,31.3541666734946,-24.3531646875));
#16708=CARTESIAN_POINT('Ctrl Pts',(48.706329375,31.1458333401613,-13.0508216223155));
#16709=CARTESIAN_POINT('Ctrl Pts',(48.706329375,30.937500006828,1.293339198242E-14));
#16710=CARTESIAN_POINT('Ctrl Pts',(48.706329375,30.7291666734946,13.0508216223155));
#16711=CARTESIAN_POINT('Ctrl Pts',(42.1809185638422,30.5208333401613,24.3531646875));
#16712=CARTESIAN_POINT('Ctrl Pts',(35.6555077526845,30.312500006828,35.6555077526845));
#16713=CARTESIAN_POINT('Ctrl Pts',(24.3531646875,30.1041666734946,42.1809185638422));
#16714=CARTESIAN_POINT('Ctrl Pts',(13.0508216223155,29.8958333401613,48.706329375));
#16715=CARTESIAN_POINT('Ctrl Pts',(-9.95098946405443E-15,29.687500006828,
48.706329375));
#16716=CARTESIAN_POINT('Ctrl Pts',(-13.0508216223155,29.4791666734946,48.706329375));
#16717=CARTESIAN_POINT('Ctrl Pts',(-24.3531646875,29.2708333401613,42.1809185638423));
#16718=CARTESIAN_POINT('Ctrl Pts',(-35.6555077526845,29.062500006828,35.6555077526845));
#16719=CARTESIAN_POINT('Ctrl Pts',(-42.1809185638422,28.8541666734946,24.3531646875));
#16720=CARTESIAN_POINT('Ctrl Pts',(-48.706329375,28.6458333401613,13.0508216223155));
#16721=CARTESIAN_POINT('Ctrl Pts',(-48.706329375,28.437500006828,-1.8898197019151E-14));
#16722=CARTESIAN_POINT('Ctrl Pts',(-46.,60.,0.));
#16723=CARTESIAN_POINT('Ctrl Pts',(-46.,59.7916666666667,-12.3256628518316));
#16724=CARTESIAN_POINT('Ctrl Pts',(-39.8371685740842,59.5833333333333,-23.));
#16725=CARTESIAN_POINT('Ctrl Pts',(-33.6743371481684,59.375,-33.6743371481684));
#16726=CARTESIAN_POINT('Ctrl Pts',(-23.,59.1666666666667,-39.8371685740842));
#16727=CARTESIAN_POINT('Ctrl Pts',(-12.3256628518317,58.9583333333333,-46.));
#16728=CARTESIAN_POINT('Ctrl Pts',(-2.81668763803891E-15,58.75,-46.));
#16729=CARTESIAN_POINT('Ctrl Pts',(12.3256628518316,58.5416666666667,-46.));
#16730=CARTESIAN_POINT('Ctrl Pts',(23.,58.3333333333333,-39.8371685740842));
#16731=CARTESIAN_POINT('Ctrl Pts',(33.6743371481683,58.125,-33.6743371481684));
#16732=CARTESIAN_POINT('Ctrl Pts',(39.8371685740842,57.9166666666667,-23.));
#16733=CARTESIAN_POINT('Ctrl Pts',(46.,57.7083333333333,-12.3256628518317));
#16734=CARTESIAN_POINT('Ctrl Pts',(46.,57.5,-5.63337527607782E-15));
#16735=CARTESIAN_POINT('Ctrl Pts',(46.,57.2916666666667,12.3256628518316));
#16736=CARTESIAN_POINT('Ctrl Pts',(39.8371685740842,57.0833333333333,23.));
#16737=CARTESIAN_POINT('Ctrl Pts',(33.6743371481684,56.875,33.6743371481683));
#16738=CARTESIAN_POINT('Ctrl Pts',(23.,56.6666666666667,39.8371685740842));
#16739=CARTESIAN_POINT('Ctrl Pts',(12.3256628518317,56.4583333333333,46.));
#16740=CARTESIAN_POINT('Ctrl Pts',(8.45006291411674E-15,56.25,46.));
#16741=CARTESIAN_POINT('Ctrl Pts',(-12.3256628518316,56.0416666666667,46.));
#16742=CARTESIAN_POINT('Ctrl Pts',(-23.,55.8333333333333,39.8371685740842));
#16743=CARTESIAN_POINT('Ctrl Pts',(-33.6743371481683,55.625,33.6743371481684));
#16744=CARTESIAN_POINT('Ctrl Pts',(-39.8371685740842,55.4166666666667,23.));
#16745=CARTESIAN_POINT('Ctrl Pts',(-46.,55.2083333333333,12.3256628518317));
#16746=CARTESIAN_POINT('Ctrl Pts',(-46.,55.,0.));
#16747=CARTESIAN_POINT('Ctrl Pts',(-46.,54.7916666666667,-12.3256628518316));
#16748=CARTESIAN_POINT('Ctrl Pts',(-39.8371685740842,54.5833333333333,-23.));
#16749=CARTESIAN_POINT('Ctrl Pts',(-33.6743371481684,54.375,-33.6743371481684));
#16750=CARTESIAN_POINT('Ctrl Pts',(-23.,54.1666666666667,-39.8371685740842));
#16751=CARTESIAN_POINT('Ctrl Pts',(-12.3256628518317,53.9583333333333,-46.));
#16752=CARTESIAN_POINT('Ctrl Pts',(-2.81668763803891E-15,53.75,-46.));
#16753=CARTESIAN_POINT('Ctrl Pts',(12.3256628518316,53.5416666666667,-46.));
#16754=CARTESIAN_POINT('Ctrl Pts',(23.,53.3333333333333,-39.8371685740842));
#16755=CARTESIAN_POINT('Ctrl Pts',(33.6743371481683,53.125,-33.6743371481684));
#16756=CARTESIAN_POINT('Ctrl Pts',(39.8371685740842,52.9166666666667,-23.));
#16757=CARTESIAN_POINT('Ctrl Pts',(46.,52.7083333333333,-12.3256628518317));
#16758=CARTESIAN_POINT('Ctrl Pts',(46.,52.5,-5.63337527607782E-15));
#16759=CARTESIAN_POINT('Ctrl Pts',(46.,52.2916666666667,12.3256628518316));
#16760=CARTESIAN_POINT('Ctrl Pts',(39.8371685740842,52.0833333333333,23.));
#16761=CARTESIAN_POINT('Ctrl Pts',(33.6743371481684,51.875,33.6743371481683));
#16762=CARTESIAN_POINT('Ctrl Pts',(23.,51.6666666666667,39.8371685740842));
#16763=CARTESIAN_POINT('Ctrl Pts',(12.3256628518317,51.4583333333333,46.));
#16764=CARTESIAN_POINT('Ctrl Pts',(8.45006291411674E-15,51.25,46.));
#16765=CARTESIAN_POINT('Ctrl Pts',(-12.3256628518316,51.0416666666667,46.));
#16766=CARTESIAN_POINT('Ctrl Pts',(-23.,50.8333333333333,39.8371685740842));
#16767=CARTESIAN_POINT('Ctrl Pts',(-33.6743371481683,50.625,33.6743371481684));
#16768=CARTESIAN_POINT('Ctrl Pts',(-39.8371685740842,50.4166666666667,23.));
#16769=CARTESIAN_POINT('Ctrl Pts',(-46.,50.2083333333333,12.3256628518317));
#16770=CARTESIAN_POINT('Ctrl Pts',(-46.,50.,0.));
#16771=CARTESIAN_POINT('Ctrl Pts',(-46.,49.7916666666667,-12.3256628518316));
#16772=CARTESIAN_POINT('Ctrl Pts',(-39.8371685740842,49.5833333333333,-23.));
#16773=CARTESIAN_POINT('Ctrl Pts',(-33.6743371481684,49.375,-33.6743371481684));
#16774=CARTESIAN_POINT('Ctrl Pts',(-23.,49.1666666666667,-39.8371685740842));
#16775=CARTESIAN_POINT('Ctrl Pts',(-12.3256628518317,48.9583333333333,-46.));
#16776=CARTESIAN_POINT('Ctrl Pts',(-2.81668763803891E-15,48.75,-46.));
#16777=CARTESIAN_POINT('Ctrl Pts',(12.3256628518316,48.5416666666667,-46.));
#16778=CARTESIAN_POINT('Ctrl Pts',(23.,48.3333333333333,-39.8371685740842));
#16779=CARTESIAN_POINT('Ctrl Pts',(33.6743371481683,48.125,-33.6743371481684));
#16780=CARTESIAN_POINT('Ctrl Pts',(39.8371685740842,47.9166666666667,-23.));
#16781=CARTESIAN_POINT('Ctrl Pts',(46.,47.7083333333333,-12.3256628518317));
#16782=CARTESIAN_POINT('Ctrl Pts',(46.,47.5,-5.63337527607782E-15));
#16783=CARTESIAN_POINT('Ctrl Pts',(46.,47.2916666666667,12.3256628518316));
#16784=CARTESIAN_POINT('Ctrl Pts',(39.8371685740842,47.0833333333333,23.));
#16785=CARTESIAN_POINT('Ctrl Pts',(33.6743371481684,46.875,33.6743371481683));
#16786=CARTESIAN_POINT('Ctrl Pts',(23.,46.6666666666667,39.8371685740842));
#16787=CARTESIAN_POINT('Ctrl Pts',(12.3256628518317,46.4583333333333,46.));
#16788=CARTESIAN_POINT('Ctrl Pts',(8.45006291411674E-15,46.25,46.));
#16789=CARTESIAN_POINT('Ctrl Pts',(-12.3256628518316,46.0416666666667,46.));
#16790=CARTESIAN_POINT('Ctrl Pts',(-23.,45.8333333333333,39.8371685740842));
#16791=CARTESIAN_POINT('Ctrl Pts',(-33.6743371481683,45.625,33.6743371481684));
#16792=CARTESIAN_POINT('Ctrl Pts',(-39.8371685740842,45.4166666666667,23.));
#16793=CARTESIAN_POINT('Ctrl Pts',(-46.,45.2083333333333,12.3256628518317));
#16794=CARTESIAN_POINT('Ctrl Pts',(-46.,45.,0.));
#16795=CARTESIAN_POINT('Ctrl Pts',(-46.,44.7916666666667,-12.3256628518316));
#16796=CARTESIAN_POINT('Ctrl Pts',(-39.8371685740842,44.5833333333333,-23.));
#16797=CARTESIAN_POINT('Ctrl Pts',(-33.6743371481684,44.375,-33.6743371481684));
#16798=CARTESIAN_POINT('Ctrl Pts',(-23.,44.1666666666667,-39.8371685740842));
#16799=CARTESIAN_POINT('Ctrl Pts',(-12.3256628518317,43.9583333333333,-46.));
#16800=CARTESIAN_POINT('Ctrl Pts',(-2.81668763803891E-15,43.75,-46.));
#16801=CARTESIAN_POINT('Ctrl Pts',(12.3256628518316,43.5416666666667,-46.));
#16802=CARTESIAN_POINT('Ctrl Pts',(23.,43.3333333333333,-39.8371685740842));
#16803=CARTESIAN_POINT('Ctrl Pts',(33.6743371481683,43.125,-33.6743371481684));
#16804=CARTESIAN_POINT('Ctrl Pts',(39.8371685740842,42.9166666666667,-23.));
#16805=CARTESIAN_POINT('Ctrl Pts',(46.,42.7083333333333,-12.3256628518317));
#16806=CARTESIAN_POINT('Ctrl Pts',(46.,42.5,-5.63337527607782E-15));
#16807=CARTESIAN_POINT('Ctrl Pts',(46.,42.2916666666667,12.3256628518316));
#16808=CARTESIAN_POINT('Ctrl Pts',(39.8371685740842,42.0833333333333,23.));
#16809=CARTESIAN_POINT('Ctrl Pts',(33.6743371481684,41.875,33.6743371481683));
#16810=CARTESIAN_POINT('Ctrl Pts',(23.,41.6666666666667,39.8371685740842));
#16811=CARTESIAN_POINT('Ctrl Pts',(12.3256628518317,41.4583333333333,46.));
#16812=CARTESIAN_POINT('Ctrl Pts',(8.45006291411674E-15,41.25,46.));
#16813=CARTESIAN_POINT('Ctrl Pts',(-12.3256628518316,41.0416666666667,46.));
#16814=CARTESIAN_POINT('Ctrl Pts',(-23.,40.8333333333333,39.8371685740842));
#16815=CARTESIAN_POINT('Ctrl Pts',(-33.6743371481683,40.625,33.6743371481684));
#16816=CARTESIAN_POINT('Ctrl Pts',(-39.8371685740842,40.4166666666667,23.));
#16817=CARTESIAN_POINT('Ctrl Pts',(-46.,40.2083333333333,12.3256628518317));
#16818=CARTESIAN_POINT('Ctrl Pts',(-46.,40.,0.));
#16819=CARTESIAN_POINT('Ctrl Pts',(-46.,39.7916666666667,-12.3256628518316));
#16820=CARTESIAN_POINT('Ctrl Pts',(-39.8371685740842,39.5833333333333,-23.));
#16821=CARTESIAN_POINT('Ctrl Pts',(-33.6743371481684,39.375,-33.6743371481684));
#16822=CARTESIAN_POINT('Ctrl Pts',(-23.,39.1666666666667,-39.8371685740842));
#16823=CARTESIAN_POINT('Ctrl Pts',(-12.3256628518317,38.9583333333333,-46.));
#16824=CARTESIAN_POINT('Ctrl Pts',(-2.81668763803891E-15,38.75,-46.));
#16825=CARTESIAN_POINT('Ctrl Pts',(12.3256628518316,38.5416666666667,-46.));
#16826=CARTESIAN_POINT('Ctrl Pts',(23.,38.3333333333333,-39.8371685740842));
#16827=CARTESIAN_POINT('Ctrl Pts',(33.6743371481683,38.125,-33.6743371481684));
#16828=CARTESIAN_POINT('Ctrl Pts',(39.8371685740842,37.9166666666667,-23.));
#16829=CARTESIAN_POINT('Ctrl Pts',(46.,37.7083333333333,-12.3256628518317));
#16830=CARTESIAN_POINT('Ctrl Pts',(46.,37.5,-5.63337527607782E-15));
#16831=CARTESIAN_POINT('Ctrl Pts',(46.,37.2916666666667,12.3256628518316));
#16832=CARTESIAN_POINT('Ctrl Pts',(39.8371685740842,37.0833333333333,23.));
#16833=CARTESIAN_POINT('Ctrl Pts',(33.6743371481684,36.875,33.6743371481683));
#16834=CARTESIAN_POINT('Ctrl Pts',(23.,36.6666666666667,39.8371685740842));
#16835=CARTESIAN_POINT('Ctrl Pts',(12.3256628518317,36.4583333333333,46.));
#16836=CARTESIAN_POINT('Ctrl Pts',(8.45006291411674E-15,36.25,46.));
#16837=CARTESIAN_POINT('Ctrl Pts',(-12.3256628518316,36.0416666666667,46.));
#16838=CARTESIAN_POINT('Ctrl Pts',(-23.,35.8333333333333,39.8371685740842));
#16839=CARTESIAN_POINT('Ctrl Pts',(-33.6743371481683,35.625,33.6743371481684));
#16840=CARTESIAN_POINT('Ctrl Pts',(-39.8371685740842,35.4166666666667,23.));
#16841=CARTESIAN_POINT('Ctrl Pts',(-46.,35.2083333333333,12.3256628518317));
#16842=CARTESIAN_POINT('Ctrl Pts',(-46.,35.,0.));
#16843=CARTESIAN_POINT('Ctrl Pts',(-46.,34.7916666666667,-12.3256628518316));
#16844=CARTESIAN_POINT('Ctrl Pts',(-39.8371685740842,34.5833333333333,-23.));
#16845=CARTESIAN_POINT('Ctrl Pts',(-33.6743371481684,34.375,-33.6743371481684));
#16846=CARTESIAN_POINT('Ctrl Pts',(-23.,34.1666666666667,-39.8371685740842));
#16847=CARTESIAN_POINT('Ctrl Pts',(-12.3256628518317,33.9583333333333,-46.));
#16848=CARTESIAN_POINT('Ctrl Pts',(-2.81668763803891E-15,33.75,-46.));
#16849=CARTESIAN_POINT('Ctrl Pts',(12.3256628518316,33.5416666666667,-46.));
#16850=CARTESIAN_POINT('Ctrl Pts',(23.,33.3333333333333,-39.8371685740842));
#16851=CARTESIAN_POINT('Ctrl Pts',(33.6743371481683,33.125,-33.6743371481684));
#16852=CARTESIAN_POINT('Ctrl Pts',(39.8371685740842,32.9166666666667,-23.));
#16853=CARTESIAN_POINT('Ctrl Pts',(46.,32.7083333333333,-12.3256628518317));
#16854=CARTESIAN_POINT('Ctrl Pts',(46.,32.5,-5.63337527607782E-15));
#16855=CARTESIAN_POINT('Ctrl Pts',(46.,32.2916666666667,12.3256628518316));
#16856=CARTESIAN_POINT('Ctrl Pts',(39.8371685740842,32.0833333333333,23.));
#16857=CARTESIAN_POINT('Ctrl Pts',(33.6743371481684,31.875,33.6743371481683));
#16858=CARTESIAN_POINT('Ctrl Pts',(23.,31.6666666666667,39.8371685740842));
#16859=CARTESIAN_POINT('Ctrl Pts',(12.3256628518317,31.4583333333333,46.));
#16860=CARTESIAN_POINT('Ctrl Pts',(8.45006291411674E-15,31.25,46.));
#16861=CARTESIAN_POINT('Ctrl Pts',(-12.3256628518316,31.0416666666667,46.));
#16862=CARTESIAN_POINT('Ctrl Pts',(-23.,30.8333333333333,39.8371685740842));
#16863=CARTESIAN_POINT('Ctrl Pts',(-33.6743371481683,30.625,33.6743371481684));
#16864=CARTESIAN_POINT('Ctrl Pts',(-39.8371685740842,30.4166666666667,23.));
#16865=CARTESIAN_POINT('Ctrl Pts',(-46.,30.2083333333333,12.3256628518317));
#16866=CARTESIAN_POINT('Ctrl Pts',(-46.,30.,0.));
#16867=CARTESIAN_POINT('Ctrl Pts',(48.5725845633798,35.8793483229262,3.60701400320329));
#16868=CARTESIAN_POINT('Ctrl Pts',(48.3407853679392,36.0125314497137,3.60701400320329));
#16869=CARTESIAN_POINT('Ctrl Pts',(48.1089821836664,36.1457076343818,3.60701400320328));
#16870=CARTESIAN_POINT('Ctrl Pts',(47.6453674864979,36.4120455056142,3.60701400320328));
#16871=CARTESIAN_POINT('Ctrl Pts',(47.4135559734254,36.5452071923974,3.60701400320326));
#16872=CARTESIAN_POINT('Ctrl Pts',(47.1817401099609,36.6783613050641,3.60701400320326));
#16873=CARTESIAN_POINT('Ctrl Pts',(46.7406305897488,36.9317328641751,3.60701400320326));
#16874=CARTESIAN_POINT('Ctrl Pts',(46.2995053259033,37.1850770165972,3.60701400320326));
#16875=CARTESIAN_POINT('Ctrl Pts',(45.858362923034,37.438391319744,3.60701400320326));
#16876=CARTESIAN_POINT('Ctrl Pts',(3.56213286848821,36.3108341932625,45.8618709760874));
#16877=CARTESIAN_POINT('Ctrl Pts',(3.51887378961017,36.0430694733184,46.3280421398764));
#16878=CARTESIAN_POINT('Ctrl Pts',(3.44742574291548,35.7751733418289,46.795680048244));
#16879=CARTESIAN_POINT('Ctrl Pts',(3.24428578910431,35.2498476701132,47.7144823615628));
#16880=CARTESIAN_POINT('Ctrl Pts',(3.11082194025322,34.987765723523,48.1737954859953));
#16881=CARTESIAN_POINT('Ctrl Pts',(2.94136876951423,34.7348340040708,48.6174338169726));
#16882=CARTESIAN_POINT('Origin',(0.,57.,0.));
#16883=CARTESIAN_POINT('',(-48.3871149493437,57.,-4.33048599679673));
#16884=CARTESIAN_POINT('',(-4.32456003949879,57.,-48.3876449370521));
#16885=CARTESIAN_POINT('Origin',(0.,57.,0.));
#16886=CARTESIAN_POINT('',(-4.32456003949879,57.,-48.3876449370521));
#16887=CARTESIAN_POINT('Origin',(0.,57.,0.));
#16888=CARTESIAN_POINT('',(0.,57.,-4.33048599679673));
#16889=CARTESIAN_POINT('',(3.61292728433799,57.,-48.4459777332189));
#16890=CARTESIAN_POINT('Origin',(0.,57.,0.));
#16891=CARTESIAN_POINT('',(3.61292728433799,57.,0.));
#16892=CARTESIAN_POINT('Origin',(0.,57.,0.));
#16893=CARTESIAN_POINT('',(0.,57.,3.60701400320327));
#16894=CARTESIAN_POINT('',(3.61292728433799,57.,45.8578974271399));
#16895=CARTESIAN_POINT('',(3.61292728433799,57.,0.));
#16896=CARTESIAN_POINT('Origin',(0.,57.,0.));
#16897=CARTESIAN_POINT('Origin',(0.,57.,0.));
#16898=CARTESIAN_POINT('',(0.,57.,-4.33048599679673));
#16899=CARTESIAN_POINT('',(-4.32456003949879,57.,0.));
#16900=CARTESIAN_POINT('Origin',(0.,57.,0.));
#16901=CARTESIAN_POINT('',(0.,57.,3.60701400320327));
#16902=CARTESIAN_POINT('',(-4.32456003949879,57.,0.));
#16903=CARTESIAN_POINT('Origin',(0.,60.,0.));
#16904=CARTESIAN_POINT('',(45.858362923034,33.0633913333999,3.60701400320327));
#16905=CARTESIAN_POINT('',(45.858362923034,32.438391319744,3.60701400320325));
#16906=CARTESIAN_POINT('',(45.858362923034,60.,3.60701400320327));
#16907=CARTESIAN_POINT('',(-45.858362923034,30.686608693912,3.60701400320327));
#16908=CARTESIAN_POINT('Ctrl Pts',(45.858362923034,33.0633913333999,3.60701400320327));
#16909=CARTESIAN_POINT('Ctrl Pts',(45.0420919829705,32.8842847836873,13.9848082063042));
#16910=CARTESIAN_POINT('Ctrl Pts',(39.8371685740842,32.7083333469893,23.));
#16911=CARTESIAN_POINT('Ctrl Pts',(33.6743371481684,32.5000000136559,33.6743371481683));
#16912=CARTESIAN_POINT('Ctrl Pts',(23.,32.2916666803226,39.8371685740842));
#16913=CARTESIAN_POINT('Ctrl Pts',(12.3256628518317,32.0833333469893,46.));
#16914=CARTESIAN_POINT('Ctrl Pts',(8.45006291411674E-15,31.8750000136559,
46.));
#16915=CARTESIAN_POINT('Ctrl Pts',(-12.3256628518316,31.6666666803226,46.));
#16916=CARTESIAN_POINT('Ctrl Pts',(-23.,31.4583333469893,39.8371685740842));
#16917=CARTESIAN_POINT('Ctrl Pts',(-33.6743371481683,31.2500000136559,33.6743371481684));
#16918=CARTESIAN_POINT('Ctrl Pts',(-39.8371685740842,31.0416666803226,23.));
#16919=CARTESIAN_POINT('Ctrl Pts',(-45.0420919829705,30.8657152436245,13.9848082063043));
#16920=CARTESIAN_POINT('Ctrl Pts',(-45.858362923034,30.686608693912,3.60701400320327));
#16921=CARTESIAN_POINT('',(-45.858362923034,30.061608680256,3.60701400320318));
#16922=CARTESIAN_POINT('',(-45.858362923034,60.,3.60701400320327));
#16923=CARTESIAN_POINT('Ctrl Pts',(45.858362923034,32.438391319744,3.60701400320325));
#16924=CARTESIAN_POINT('Ctrl Pts',(45.0420919829705,32.2592847700314,13.9848082063042));
#16925=CARTESIAN_POINT('Ctrl Pts',(39.8371685740842,32.0833333333333,23.));
#16926=CARTESIAN_POINT('Ctrl Pts',(33.6743371481684,31.875,33.6743371481683));
#16927=CARTESIAN_POINT('Ctrl Pts',(23.,31.6666666666667,39.8371685740842));
#16928=CARTESIAN_POINT('Ctrl Pts',(12.3256628518317,31.4583333333333,46.));
#16929=CARTESIAN_POINT('Ctrl Pts',(8.45006291411674E-15,31.25,46.));
#16930=CARTESIAN_POINT('Ctrl Pts',(-12.3256628518316,31.0416666666667,46.));
#16931=CARTESIAN_POINT('Ctrl Pts',(-23.,30.8333333333333,39.8371685740842));
#16932=CARTESIAN_POINT('Ctrl Pts',(-33.6743371481683,30.625,33.6743371481684));
#16933=CARTESIAN_POINT('Ctrl Pts',(-39.8371685740842,30.4166666666667,23.));
#16934=CARTESIAN_POINT('Ctrl Pts',(-45.0420919829705,30.2407152299686,13.9848082063043));
#16935=CARTESIAN_POINT('Ctrl Pts',(-45.858362923034,30.061608680256,3.60701400320318));
#16936=CARTESIAN_POINT('Origin',(0.,60.,0.));
#16937=CARTESIAN_POINT('',(45.7957082162897,32.5741208584476,-4.33048599679664));
#16938=CARTESIAN_POINT('',(45.7957082162897,33.1991208721035,-4.33048599679673));
#16939=CARTESIAN_POINT('',(45.7957082162897,60.,-4.33048599679673));
#16940=CARTESIAN_POINT('',(1.95443836226898,33.7167771652757,-45.9584613611911));
#16941=CARTESIAN_POINT('Ctrl Pts',(1.95443836226898,33.7167771652757,-45.9584613611911));
#16942=CARTESIAN_POINT('Ctrl Pts',(13.2279919463142,33.5240557157094,-45.4790400544029));
#16943=CARTESIAN_POINT('Ctrl Pts',(23.,33.3333333333333,-39.8371685740842));
#16944=CARTESIAN_POINT('Ctrl Pts',(33.6743371481683,33.125,-33.6743371481684));
#16945=CARTESIAN_POINT('Ctrl Pts',(39.8371685740842,32.9166666666667,-23.));
#16946=CARTESIAN_POINT('Ctrl Pts',(44.8515840435634,32.7471553142902,-14.3147776366026));
#16947=CARTESIAN_POINT('Ctrl Pts',(45.7957082162897,32.5741208584476,-4.33048599679664));
#16948=CARTESIAN_POINT('',(2.63082218623052,34.3301917962911,-45.9247076705387));
#16949=CARTESIAN_POINT('Ctrl Pts',(2.6308221862305,34.3301917962911,-45.9247076705387));
#16950=CARTESIAN_POINT('Ctrl Pts',(2.56921791197849,34.2597950751581,-45.928236705337));
#16951=CARTESIAN_POINT('Ctrl Pts',(2.50510731292546,34.1915500441504,-45.9317853835034));
#16952=CARTESIAN_POINT('Ctrl Pts',(2.43846309439405,34.1254745197606,-45.9353231235497));
#16953=CARTESIAN_POINT('Ctrl Pts',(2.3971217800392,34.0844859826429,-45.9375176848572));
#16954=CARTESIAN_POINT('Ctrl Pts',(2.35480478224494,34.0443330034482,-45.9397080370933));
#16955=CARTESIAN_POINT('Ctrl Pts',(2.31149948807074,34.0050278948341,-45.9418868802387));
#16956=CARTESIAN_POINT('Ctrl Pts',(2.26335270074926,33.9613285102397,-45.9443093160985));
#16957=CARTESIAN_POINT('Ctrl Pts',(2.21394822234029,33.9186513826451,-45.946718418332));
#16958=CARTESIAN_POINT('Ctrl Pts',(2.16351946109064,33.8772218703134,-45.9490927134335));
#16959=CARTESIAN_POINT('Ctrl Pts',(2.11305915068249,33.8357664389186,-45.9514684939376));
#16960=CARTESIAN_POINT('Ctrl Pts',(2.06157358891504,33.7955604486027,-45.9538094237443));
#16961=CARTESIAN_POINT('Ctrl Pts',(2.00932978732685,33.7567892931775,-45.95609398902));
#16962=CARTESIAN_POINT('Ctrl Pts',(1.99112044191851,33.7432757788551,-45.9568902641177));
#16963=CARTESIAN_POINT('Ctrl Pts',(1.97281925470307,33.7299361972055,-45.9576796918261));
#16964=CARTESIAN_POINT('Ctrl Pts',(1.95443836226869,33.7167771652761,-45.9584613611911));
#16965=CARTESIAN_POINT('Ctrl Pts',(2.63082218623052,34.3301917962911,-45.9247076705387));
#16966=CARTESIAN_POINT('Ctrl Pts',(13.5383323474866,34.1429987490258,-45.2998649402456));
#16967=CARTESIAN_POINT('Ctrl Pts',(23.,33.9583333469893,-39.8371685740842));
#16968=CARTESIAN_POINT('Ctrl Pts',(33.6743371481683,33.7500000136559,-33.6743371481684));
#16969=CARTESIAN_POINT('Ctrl Pts',(39.8371685740842,33.5416666803226,-23.));
#16970=CARTESIAN_POINT('Ctrl Pts',(44.8515840435634,33.3721553279462,-14.3147776366027));
#16971=CARTESIAN_POINT('Ctrl Pts',(45.7957082162897,33.1991208721035,-4.33048599679673));
#16972=CARTESIAN_POINT('Origin',(0.,60.,0.));
#16973=CARTESIAN_POINT('',(-45.7957082162897,34.9258791415524,-4.33048599679682));
#16974=CARTESIAN_POINT('',(-45.7957082162897,60.,-4.33048599679673));
#16975=CARTESIAN_POINT('',(-2.77456427460704,33.7972761197826,-45.9162475937012));
#16976=CARTESIAN_POINT('Ctrl Pts',(-2.77456427460705,33.7972761197826,-45.9162475937012));
#16977=CARTESIAN_POINT('Ctrl Pts',(-2.8485761476615,33.8541693341362,-45.9117753053581));
#16978=CARTESIAN_POINT('Ctrl Pts',(-2.92014445685112,33.9133331099627,-45.9072715943004));
#16979=CARTESIAN_POINT('Ctrl Pts',(-2.98933369598369,33.9747022029095,-45.9027657035543));
#16980=CARTESIAN_POINT('Ctrl Pts',(-3.03440838807543,34.0146823067985,-45.8998302523118));
#16981=CARTESIAN_POINT('Ctrl Pts',(-3.07847297023139,34.0555994041398,-45.8968938759819));
#16982=CARTESIAN_POINT('Ctrl Pts',(-3.12153932925008,34.0974457295403,-45.8939646600285));
#16983=CARTESIAN_POINT('Ctrl Pts',(-3.1893556202593,34.1633408422383,-45.8893520443803));
#16984=CARTESIAN_POINT('Ctrl Pts',(-3.25469619442314,34.2315362288938,-45.8847569569152));
#16985=CARTESIAN_POINT('Ctrl Pts',(-3.31757026199471,34.3020256949546,-45.8802105832609));
#16986=CARTESIAN_POINT('Ctrl Pts',(-3.35591287101332,34.3450124165315,-45.8774380597992));
#16987=CARTESIAN_POINT('Ctrl Pts',(-3.39333752726835,34.3888530647444,-45.8746836527545));
#16988=CARTESIAN_POINT('Ctrl Pts',(-3.42983911135813,34.4335524565479,-45.87195443482));
#16989=CARTESIAN_POINT('Ctrl Pts',(-45.7957082162897,34.9258791415524,-4.33048599679682));
#16990=CARTESIAN_POINT('Ctrl Pts',(-44.8515840435634,34.7528446857097,-14.3147776366027));
#16991=CARTESIAN_POINT('Ctrl Pts',(-39.8371685740842,34.5833333333333,-23.));
#16992=CARTESIAN_POINT('Ctrl Pts',(-33.6743371481684,34.375,-33.6743371481684));
#16993=CARTESIAN_POINT('Ctrl Pts',(-23.,34.1666666666667,-39.8371685740842));
#16994=CARTESIAN_POINT('Ctrl Pts',(-13.6041749881978,33.9832863296065,-45.2618506739068));
#16995=CARTESIAN_POINT('Ctrl Pts',(-2.77456427460704,33.7972761197826,-45.9162475937012));
#16996=CARTESIAN_POINT('Origin',(0.,60.,0.));
#16997=CARTESIAN_POINT('',(-45.858362923034,35.061608680256,3.60701400320325));
#16998=CARTESIAN_POINT('',(-45.858362923034,60.,3.60701400320327));
#16999=CARTESIAN_POINT('',(-4.24983907177925,36.1772764823076,45.8032626333974));
#17000=CARTESIAN_POINT('Ctrl Pts',(-4.24983907177925,36.1772764823076,45.8032626333974));
#17001=CARTESIAN_POINT('Ctrl Pts',(-14.2780294172147,36.0035619086092,44.8728006379193));
#17002=CARTESIAN_POINT('Ctrl Pts',(-23.,35.8333333333333,39.8371685740842));
#17003=CARTESIAN_POINT('Ctrl Pts',(-33.6743371481683,35.625,33.6743371481684));
#17004=CARTESIAN_POINT('Ctrl Pts',(-39.8371685740842,35.4166666666667,23.));
#17005=CARTESIAN_POINT('Ctrl Pts',(-45.0420919829705,35.2407152299686,13.9848082063043));
#17006=CARTESIAN_POINT('Ctrl Pts',(-45.858362923034,35.061608680256,3.60701400320325));
#17007=CARTESIAN_POINT('Ctrl Pts',(-4.32199731091473,36.8010262662206,45.796510120799));
#17008=CARTESIAN_POINT('Ctrl Pts',(-4.31460736934614,36.5957426618924,45.7972075387355));
#17009=CARTESIAN_POINT('Ctrl Pts',(-4.29092724654331,36.3860078913526,45.7994502820394));
#17010=CARTESIAN_POINT('Ctrl Pts',(-4.24983907177925,36.1772764823076,45.8032626333974));
#17011=CARTESIAN_POINT('Ctrl Pts',(-46.,55.6250000136559,0.));
#17012=CARTESIAN_POINT('Ctrl Pts',(-46.,55.4166666803226,-12.3256628518316));
#17013=CARTESIAN_POINT('Ctrl Pts',(-39.8371685740842,55.2083333469893,-23.));
#17014=CARTESIAN_POINT('Ctrl Pts',(-33.6743371481684,55.0000000136559,-33.6743371481684));
#17015=CARTESIAN_POINT('Ctrl Pts',(-23.,54.7916666803226,-39.8371685740842));
#17016=CARTESIAN_POINT('Ctrl Pts',(-12.3256628518317,54.5833333469893,-46.));
#17017=CARTESIAN_POINT('Ctrl Pts',(-2.81668763803891E-15,54.3750000136559,
-46.));
#17018=CARTESIAN_POINT('Ctrl Pts',(12.3256628518316,54.1666666803226,-46.));
#17019=CARTESIAN_POINT('Ctrl Pts',(23.,53.9583333469893,-39.8371685740842));
#17020=CARTESIAN_POINT('Ctrl Pts',(33.6743371481683,53.7500000136559,-33.6743371481684));
#17021=CARTESIAN_POINT('Ctrl Pts',(39.8371685740842,53.5416666803226,-23.));
#17022=CARTESIAN_POINT('Ctrl Pts',(46.,53.3333333469893,-12.3256628518317));
#17023=CARTESIAN_POINT('Ctrl Pts',(46.,53.1250000136559,-5.63337527607782E-15));
#17024=CARTESIAN_POINT('Ctrl Pts',(46.,52.9166666803226,12.3256628518316));
#17025=CARTESIAN_POINT('Ctrl Pts',(39.8371685740842,52.7083333469893,23.));
#17026=CARTESIAN_POINT('Ctrl Pts',(33.6743371481684,52.5000000136559,33.6743371481683));
#17027=CARTESIAN_POINT('Ctrl Pts',(23.,52.2916666803226,39.8371685740842));
#17028=CARTESIAN_POINT('Ctrl Pts',(12.3256628518317,52.0833333469893,46.));
#17029=CARTESIAN_POINT('Ctrl Pts',(8.45006291411674E-15,51.8750000136559,
46.));
#17030=CARTESIAN_POINT('Ctrl Pts',(-12.3256628518316,51.6666666803226,46.));
#17031=CARTESIAN_POINT('Ctrl Pts',(-23.,51.4583333469893,39.8371685740842));
#17032=CARTESIAN_POINT('Ctrl Pts',(-33.6743371481683,51.2500000136559,33.6743371481684));
#17033=CARTESIAN_POINT('Ctrl Pts',(-39.8371685740842,51.0416666803226,23.));
#17034=CARTESIAN_POINT('Ctrl Pts',(-46.,50.8333333469893,12.3256628518317));
#17035=CARTESIAN_POINT('Ctrl Pts',(-46.,50.6250000136559,0.));
#17036=CARTESIAN_POINT('Ctrl Pts',(-46.,50.4166666803226,-12.3256628518316));
#17037=CARTESIAN_POINT('Ctrl Pts',(-39.8371685740842,50.2083333469893,-23.));
#17038=CARTESIAN_POINT('Ctrl Pts',(-33.6743371481684,50.0000000136559,-33.6743371481684));
#17039=CARTESIAN_POINT('Ctrl Pts',(-23.,49.7916666803226,-39.8371685740842));
#17040=CARTESIAN_POINT('Ctrl Pts',(-12.3256628518317,49.5833333469893,-46.));
#17041=CARTESIAN_POINT('Ctrl Pts',(-2.81668763803891E-15,49.3750000136559,
-46.));
#17042=CARTESIAN_POINT('Ctrl Pts',(12.3256628518316,49.1666666803226,-46.));
#17043=CARTESIAN_POINT('Ctrl Pts',(23.,48.9583333469893,-39.8371685740842));
#17044=CARTESIAN_POINT('Ctrl Pts',(33.6743371481683,48.7500000136559,-33.6743371481684));
#17045=CARTESIAN_POINT('Ctrl Pts',(39.8371685740842,48.5416666803226,-23.));
#17046=CARTESIAN_POINT('Ctrl Pts',(46.,48.3333333469893,-12.3256628518317));
#17047=CARTESIAN_POINT('Ctrl Pts',(46.,48.1250000136559,-5.63337527607782E-15));
#17048=CARTESIAN_POINT('Ctrl Pts',(46.,47.9166666803226,12.3256628518316));
#17049=CARTESIAN_POINT('Ctrl Pts',(39.8371685740842,47.7083333469893,23.));
#17050=CARTESIAN_POINT('Ctrl Pts',(33.6743371481684,47.5000000136559,33.6743371481683));
#17051=CARTESIAN_POINT('Ctrl Pts',(23.,47.2916666803226,39.8371685740842));
#17052=CARTESIAN_POINT('Ctrl Pts',(12.3256628518317,47.0833333469893,46.));
#17053=CARTESIAN_POINT('Ctrl Pts',(8.45006291411674E-15,46.8750000136559,
46.));
#17054=CARTESIAN_POINT('Ctrl Pts',(-12.3256628518316,46.6666666803226,46.));
#17055=CARTESIAN_POINT('Ctrl Pts',(-23.,46.4583333469893,39.8371685740842));
#17056=CARTESIAN_POINT('Ctrl Pts',(-33.6743371481683,46.2500000136559,33.6743371481684));
#17057=CARTESIAN_POINT('Ctrl Pts',(-39.8371685740842,46.0416666803226,23.));
#17058=CARTESIAN_POINT('Ctrl Pts',(-46.,45.8333333469892,12.3256628518317));
#17059=CARTESIAN_POINT('Ctrl Pts',(-46.,45.6250000136559,0.));
#17060=CARTESIAN_POINT('Ctrl Pts',(-46.,45.4166666803226,-12.3256628518316));
#17061=CARTESIAN_POINT('Ctrl Pts',(-39.8371685740842,45.2083333469893,-23.));
#17062=CARTESIAN_POINT('Ctrl Pts',(-33.6743371481684,45.0000000136559,-33.6743371481684));
#17063=CARTESIAN_POINT('Ctrl Pts',(-23.,44.7916666803226,-39.8371685740842));
#17064=CARTESIAN_POINT('Ctrl Pts',(-12.3256628518317,44.5833333469893,-46.));
#17065=CARTESIAN_POINT('Ctrl Pts',(-2.81668763803891E-15,44.3750000136559,
-46.));
#17066=CARTESIAN_POINT('Ctrl Pts',(12.3256628518316,44.1666666803226,-46.));
#17067=CARTESIAN_POINT('Ctrl Pts',(23.,43.9583333469893,-39.8371685740842));
#17068=CARTESIAN_POINT('Ctrl Pts',(33.6743371481683,43.7500000136559,-33.6743371481684));
#17069=CARTESIAN_POINT('Ctrl Pts',(39.8371685740842,43.5416666803226,-23.));
#17070=CARTESIAN_POINT('Ctrl Pts',(46.,43.3333333469893,-12.3256628518317));
#17071=CARTESIAN_POINT('Ctrl Pts',(46.,43.1250000136559,-5.63337527607782E-15));
#17072=CARTESIAN_POINT('Ctrl Pts',(46.,42.9166666803226,12.3256628518316));
#17073=CARTESIAN_POINT('Ctrl Pts',(39.8371685740842,42.7083333469893,23.));
#17074=CARTESIAN_POINT('Ctrl Pts',(33.6743371481684,42.5000000136559,33.6743371481683));
#17075=CARTESIAN_POINT('Ctrl Pts',(23.,42.2916666803226,39.8371685740842));
#17076=CARTESIAN_POINT('Ctrl Pts',(12.3256628518317,42.0833333469893,46.));
#17077=CARTESIAN_POINT('Ctrl Pts',(8.45006291411674E-15,41.8750000136559,
46.));
#17078=CARTESIAN_POINT('Ctrl Pts',(-12.3256628518316,41.6666666803226,46.));
#17079=CARTESIAN_POINT('Ctrl Pts',(-23.,41.4583333469893,39.8371685740842));
#17080=CARTESIAN_POINT('Ctrl Pts',(-33.6743371481683,41.2500000136559,33.6743371481684));
#17081=CARTESIAN_POINT('Ctrl Pts',(-39.8371685740842,41.0416666803226,23.));
#17082=CARTESIAN_POINT('Ctrl Pts',(-46.,40.8333333469893,12.3256628518317));
#17083=CARTESIAN_POINT('Ctrl Pts',(-46.,40.6250000136559,0.));
#17084=CARTESIAN_POINT('Ctrl Pts',(-46.,40.4166666803226,-12.3256628518316));
#17085=CARTESIAN_POINT('Ctrl Pts',(-39.8371685740842,40.2083333469893,-23.));
#17086=CARTESIAN_POINT('Ctrl Pts',(-33.6743371481684,40.0000000136559,-33.6743371481684));
#17087=CARTESIAN_POINT('Ctrl Pts',(-23.,39.7916666803226,-39.8371685740842));
#17088=CARTESIAN_POINT('Ctrl Pts',(-12.3256628518317,39.5833333469893,-46.));
#17089=CARTESIAN_POINT('Ctrl Pts',(-2.81668763803891E-15,39.3750000136559,
-46.));
#17090=CARTESIAN_POINT('Ctrl Pts',(12.3256628518316,39.1666666803226,-46.));
#17091=CARTESIAN_POINT('Ctrl Pts',(23.,38.9583333469893,-39.8371685740842));
#17092=CARTESIAN_POINT('Ctrl Pts',(33.6743371481683,38.7500000136559,-33.6743371481684));
#17093=CARTESIAN_POINT('Ctrl Pts',(39.8371685740842,38.5416666803226,-23.));
#17094=CARTESIAN_POINT('Ctrl Pts',(46.,38.3333333469893,-12.3256628518317));
#17095=CARTESIAN_POINT('Ctrl Pts',(46.,38.1250000136559,-5.63337527607782E-15));
#17096=CARTESIAN_POINT('Ctrl Pts',(46.,37.9166666803226,12.3256628518316));
#17097=CARTESIAN_POINT('Ctrl Pts',(39.8371685740842,37.7083333469893,23.));
#17098=CARTESIAN_POINT('Ctrl Pts',(33.6743371481684,37.5000000136559,33.6743371481683));
#17099=CARTESIAN_POINT('Ctrl Pts',(23.,37.2916666803226,39.8371685740842));
#17100=CARTESIAN_POINT('Ctrl Pts',(12.3256628518317,37.0833333469893,46.));
#17101=CARTESIAN_POINT('Ctrl Pts',(8.45006291411674E-15,36.8750000136559,
46.));
#17102=CARTESIAN_POINT('Ctrl Pts',(-12.3256628518316,36.6666666803226,46.));
#17103=CARTESIAN_POINT('Ctrl Pts',(-23.,36.4583333469893,39.8371685740842));
#17104=CARTESIAN_POINT('Ctrl Pts',(-33.6743371481683,36.2500000136559,33.6743371481684));
#17105=CARTESIAN_POINT('Ctrl Pts',(-39.8371685740842,36.0416666803226,23.));
#17106=CARTESIAN_POINT('Ctrl Pts',(-46.,35.8333333469893,12.3256628518317));
#17107=CARTESIAN_POINT('Ctrl Pts',(-46.,35.6250000136559,0.));
#17108=CARTESIAN_POINT('Ctrl Pts',(-46.,35.4166666803226,-12.3256628518316));
#17109=CARTESIAN_POINT('Ctrl Pts',(-39.8371685740842,35.2083333469893,-23.));
#17110=CARTESIAN_POINT('Ctrl Pts',(-33.6743371481684,35.0000000136559,-33.6743371481684));
#17111=CARTESIAN_POINT('Ctrl Pts',(-23.,34.7916666803226,-39.8371685740842));
#17112=CARTESIAN_POINT('Ctrl Pts',(-12.3256628518317,34.5833333469893,-46.));
#17113=CARTESIAN_POINT('Ctrl Pts',(-2.81668763803891E-15,34.3750000136559,
-46.));
#17114=CARTESIAN_POINT('Ctrl Pts',(12.3256628518316,34.1666666803226,-46.));
#17115=CARTESIAN_POINT('Ctrl Pts',(23.,33.9583333469893,-39.8371685740842));
#17116=CARTESIAN_POINT('Ctrl Pts',(33.6743371481683,33.7500000136559,-33.6743371481684));
#17117=CARTESIAN_POINT('Ctrl Pts',(39.8371685740842,33.5416666803226,-23.));
#17118=CARTESIAN_POINT('Ctrl Pts',(46.,33.3333333469893,-12.3256628518317));
#17119=CARTESIAN_POINT('Ctrl Pts',(46.,33.1250000136559,-5.63337527607782E-15));
#17120=CARTESIAN_POINT('Ctrl Pts',(46.,32.9166666803226,12.3256628518316));
#17121=CARTESIAN_POINT('Ctrl Pts',(39.8371685740842,32.7083333469893,23.));
#17122=CARTESIAN_POINT('Ctrl Pts',(33.6743371481684,32.5000000136559,33.6743371481683));
#17123=CARTESIAN_POINT('Ctrl Pts',(23.,32.2916666803226,39.8371685740842));
#17124=CARTESIAN_POINT('Ctrl Pts',(12.3256628518317,32.0833333469893,46.));
#17125=CARTESIAN_POINT('Ctrl Pts',(8.45006291411674E-15,31.8750000136559,
46.));
#17126=CARTESIAN_POINT('Ctrl Pts',(-12.3256628518316,31.6666666803226,46.));
#17127=CARTESIAN_POINT('Ctrl Pts',(-23.,31.4583333469893,39.8371685740842));
#17128=CARTESIAN_POINT('Ctrl Pts',(-33.6743371481683,31.2500000136559,33.6743371481684));
#17129=CARTESIAN_POINT('Ctrl Pts',(-39.8371685740842,31.0416666803226,23.));
#17130=CARTESIAN_POINT('Ctrl Pts',(-46.,30.8333333469893,12.3256628518317));
#17131=CARTESIAN_POINT('Ctrl Pts',(-46.,30.6250000136559,0.));
#17132=CARTESIAN_POINT('Ctrl Pts',(-46.,30.4166666803226,-12.3256628518316));
#17133=CARTESIAN_POINT('Ctrl Pts',(-39.8371685740842,30.2083333469893,-23.));
#17134=CARTESIAN_POINT('Ctrl Pts',(-33.6743371481684,30.0000000136559,-33.6743371481684));
#17135=CARTESIAN_POINT('Ctrl Pts',(-23.,29.7916666803226,-39.8371685740842));
#17136=CARTESIAN_POINT('Ctrl Pts',(-12.3256628518317,29.5833333469893,-46.));
#17137=CARTESIAN_POINT('Ctrl Pts',(-2.81668763803891E-15,29.3750000136559,
-46.));
#17138=CARTESIAN_POINT('Ctrl Pts',(12.3256628518316,29.1666666803226,-46.));
#17139=CARTESIAN_POINT('Ctrl Pts',(23.,28.9583333469893,-39.8371685740842));
#17140=CARTESIAN_POINT('Ctrl Pts',(33.6743371481683,28.7500000136559,-33.6743371481684));
#17141=CARTESIAN_POINT('Ctrl Pts',(39.8371685740842,28.5416666803226,-23.));
#17142=CARTESIAN_POINT('Ctrl Pts',(46.,28.3333333469893,-12.3256628518317));
#17143=CARTESIAN_POINT('Ctrl Pts',(46.,28.1250000136559,-5.63337527607782E-15));
#17144=CARTESIAN_POINT('Ctrl Pts',(46.,27.9166666803226,12.3256628518316));
#17145=CARTESIAN_POINT('Ctrl Pts',(39.8371685740842,27.7083333469893,23.));
#17146=CARTESIAN_POINT('Ctrl Pts',(33.6743371481684,27.5000000136559,33.6743371481683));
#17147=CARTESIAN_POINT('Ctrl Pts',(23.,27.2916666803226,39.8371685740842));
#17148=CARTESIAN_POINT('Ctrl Pts',(12.3256628518317,27.0833333469893,46.));
#17149=CARTESIAN_POINT('Ctrl Pts',(8.45006291411674E-15,26.8750000136559,
46.));
#17150=CARTESIAN_POINT('Ctrl Pts',(-12.3256628518316,26.6666666803226,46.));
#17151=CARTESIAN_POINT('Ctrl Pts',(-23.,26.4583333469893,39.8371685740842));
#17152=CARTESIAN_POINT('Ctrl Pts',(-33.6743371481683,26.2500000136559,33.6743371481684));
#17153=CARTESIAN_POINT('Ctrl Pts',(-39.8371685740842,26.0416666803226,23.));
#17154=CARTESIAN_POINT('Ctrl Pts',(-46.,25.8333333469893,12.3256628518317));
#17155=CARTESIAN_POINT('Ctrl Pts',(-46.,25.6250000136559,0.));
#17156=CARTESIAN_POINT('Ctrl Pts',(-48.706329375,57.187500006828,-1.8898197019151E-14));
#17157=CARTESIAN_POINT('Ctrl Pts',(-48.706329375,56.9791666734946,-13.0508216223155));
#17158=CARTESIAN_POINT('Ctrl Pts',(-42.1809185638422,56.7708333401613,-24.3531646875));
#17159=CARTESIAN_POINT('Ctrl Pts',(-35.6555077526845,56.562500006828,-35.6555077526845));
#17160=CARTESIAN_POINT('Ctrl Pts',(-24.3531646875,56.3541666734946,-42.1809185638423));
#17161=CARTESIAN_POINT('Ctrl Pts',(-13.0508216223155,56.1458333401613,-48.706329375));
#17162=CARTESIAN_POINT('Ctrl Pts',(1.59157945007855E-14,55.937500006828,
-48.706329375));
#17163=CARTESIAN_POINT('Ctrl Pts',(13.0508216223155,55.7291666734946,-48.706329375));
#17164=CARTESIAN_POINT('Ctrl Pts',(24.3531646875,55.5208333401613,-42.1809185638422));
#17165=CARTESIAN_POINT('Ctrl Pts',(35.6555077526845,55.312500006828,-35.6555077526845));
#17166=CARTESIAN_POINT('Ctrl Pts',(42.1809185638422,55.1041666734946,-24.3531646875));
#17167=CARTESIAN_POINT('Ctrl Pts',(48.706329375,54.8958333401613,-13.0508216223155));
#17168=CARTESIAN_POINT('Ctrl Pts',(48.706329375,54.687500006828,1.293339198242E-14));
#17169=CARTESIAN_POINT('Ctrl Pts',(48.706329375,54.4791666734946,13.0508216223155));
#17170=CARTESIAN_POINT('Ctrl Pts',(42.1809185638422,54.2708333401613,24.3531646875));
#17171=CARTESIAN_POINT('Ctrl Pts',(35.6555077526845,54.062500006828,35.6555077526845));
#17172=CARTESIAN_POINT('Ctrl Pts',(24.3531646875,53.8541666734946,42.1809185638422));
#17173=CARTESIAN_POINT('Ctrl Pts',(13.0508216223155,53.6458333401613,48.706329375));
#17174=CARTESIAN_POINT('Ctrl Pts',(-9.95098946405443E-15,53.437500006828,
48.706329375));
#17175=CARTESIAN_POINT('Ctrl Pts',(-13.0508216223155,53.2291666734946,48.706329375));
#17176=CARTESIAN_POINT('Ctrl Pts',(-24.3531646875,53.0208333401613,42.1809185638423));
#17177=CARTESIAN_POINT('Ctrl Pts',(-35.6555077526845,52.812500006828,35.6555077526845));
#17178=CARTESIAN_POINT('Ctrl Pts',(-42.1809185638422,52.6041666734946,24.3531646875));
#17179=CARTESIAN_POINT('Ctrl Pts',(-48.706329375,52.3958333401613,13.0508216223155));
#17180=CARTESIAN_POINT('Ctrl Pts',(-48.706329375,52.187500006828,-1.8898197019151E-14));
#17181=CARTESIAN_POINT('Ctrl Pts',(-48.706329375,51.9791666734946,-13.0508216223155));
#17182=CARTESIAN_POINT('Ctrl Pts',(-42.1809185638422,51.7708333401613,-24.3531646875));
#17183=CARTESIAN_POINT('Ctrl Pts',(-35.6555077526845,51.562500006828,-35.6555077526845));
#17184=CARTESIAN_POINT('Ctrl Pts',(-24.3531646875,51.3541666734946,-42.1809185638423));
#17185=CARTESIAN_POINT('Ctrl Pts',(-13.0508216223155,51.1458333401613,-48.706329375));
#17186=CARTESIAN_POINT('Ctrl Pts',(1.59157945007855E-14,50.937500006828,
-48.706329375));
#17187=CARTESIAN_POINT('Ctrl Pts',(13.0508216223155,50.7291666734946,-48.706329375));
#17188=CARTESIAN_POINT('Ctrl Pts',(24.3531646875,50.5208333401613,-42.1809185638422));
#17189=CARTESIAN_POINT('Ctrl Pts',(35.6555077526845,50.312500006828,-35.6555077526845));
#17190=CARTESIAN_POINT('Ctrl Pts',(42.1809185638422,50.1041666734946,-24.3531646875));
#17191=CARTESIAN_POINT('Ctrl Pts',(48.706329375,49.8958333401613,-13.0508216223155));
#17192=CARTESIAN_POINT('Ctrl Pts',(48.706329375,49.687500006828,1.293339198242E-14));
#17193=CARTESIAN_POINT('Ctrl Pts',(48.706329375,49.4791666734946,13.0508216223155));
#17194=CARTESIAN_POINT('Ctrl Pts',(42.1809185638422,49.2708333401613,24.3531646875));
#17195=CARTESIAN_POINT('Ctrl Pts',(35.6555077526845,49.062500006828,35.6555077526845));
#17196=CARTESIAN_POINT('Ctrl Pts',(24.3531646875,48.8541666734946,42.1809185638422));
#17197=CARTESIAN_POINT('Ctrl Pts',(13.0508216223155,48.6458333401613,48.706329375));
#17198=CARTESIAN_POINT('Ctrl Pts',(-9.95098946405443E-15,48.437500006828,
48.706329375));
#17199=CARTESIAN_POINT('Ctrl Pts',(-13.0508216223155,48.2291666734946,48.706329375));
#17200=CARTESIAN_POINT('Ctrl Pts',(-24.3531646875,48.0208333401613,42.1809185638423));
#17201=CARTESIAN_POINT('Ctrl Pts',(-35.6555077526845,47.812500006828,35.6555077526845));
#17202=CARTESIAN_POINT('Ctrl Pts',(-42.1809185638422,47.6041666734946,24.3531646875));
#17203=CARTESIAN_POINT('Ctrl Pts',(-48.706329375,47.3958333401613,13.0508216223155));
#17204=CARTESIAN_POINT('Ctrl Pts',(-48.706329375,47.187500006828,-1.8898197019151E-14));
#17205=CARTESIAN_POINT('Ctrl Pts',(-48.706329375,46.9791666734946,-13.0508216223155));
#17206=CARTESIAN_POINT('Ctrl Pts',(-42.1809185638422,46.7708333401613,-24.3531646875));
#17207=CARTESIAN_POINT('Ctrl Pts',(-35.6555077526845,46.562500006828,-35.6555077526845));
#17208=CARTESIAN_POINT('Ctrl Pts',(-24.3531646875,46.3541666734946,-42.1809185638423));
#17209=CARTESIAN_POINT('Ctrl Pts',(-13.0508216223155,46.1458333401613,-48.706329375));
#17210=CARTESIAN_POINT('Ctrl Pts',(1.59157945007855E-14,45.937500006828,
-48.706329375));
#17211=CARTESIAN_POINT('Ctrl Pts',(13.0508216223155,45.7291666734946,-48.706329375));
#17212=CARTESIAN_POINT('Ctrl Pts',(24.3531646875,45.5208333401613,-42.1809185638422));
#17213=CARTESIAN_POINT('Ctrl Pts',(35.6555077526845,45.312500006828,-35.6555077526845));
#17214=CARTESIAN_POINT('Ctrl Pts',(42.1809185638422,45.1041666734946,-24.3531646875));
#17215=CARTESIAN_POINT('Ctrl Pts',(48.706329375,44.8958333401613,-13.0508216223155));
#17216=CARTESIAN_POINT('Ctrl Pts',(48.706329375,44.687500006828,1.293339198242E-14));
#17217=CARTESIAN_POINT('Ctrl Pts',(48.706329375,44.4791666734946,13.0508216223155));
#17218=CARTESIAN_POINT('Ctrl Pts',(42.1809185638422,44.2708333401613,24.3531646875));
#17219=CARTESIAN_POINT('Ctrl Pts',(35.6555077526845,44.062500006828,35.6555077526845));
#17220=CARTESIAN_POINT('Ctrl Pts',(24.3531646875,43.8541666734946,42.1809185638422));
#17221=CARTESIAN_POINT('Ctrl Pts',(13.0508216223155,43.6458333401613,48.706329375));
#17222=CARTESIAN_POINT('Ctrl Pts',(-9.95098946405443E-15,43.437500006828,
48.706329375));
#17223=CARTESIAN_POINT('Ctrl Pts',(-13.0508216223155,43.2291666734946,48.706329375));
#17224=CARTESIAN_POINT('Ctrl Pts',(-24.3531646875,43.0208333401613,42.1809185638423));
#17225=CARTESIAN_POINT('Ctrl Pts',(-35.6555077526845,42.812500006828,35.6555077526845));
#17226=CARTESIAN_POINT('Ctrl Pts',(-42.1809185638422,42.6041666734946,24.3531646875));
#17227=CARTESIAN_POINT('Ctrl Pts',(-48.706329375,42.3958333401613,13.0508216223155));
#17228=CARTESIAN_POINT('Ctrl Pts',(-48.706329375,42.187500006828,-1.8898197019151E-14));
#17229=CARTESIAN_POINT('Ctrl Pts',(-48.706329375,41.9791666734946,-13.0508216223155));
#17230=CARTESIAN_POINT('Ctrl Pts',(-42.1809185638422,41.7708333401613,-24.3531646875));
#17231=CARTESIAN_POINT('Ctrl Pts',(-35.6555077526845,41.562500006828,-35.6555077526845));
#17232=CARTESIAN_POINT('Ctrl Pts',(-24.3531646875,41.3541666734946,-42.1809185638423));
#17233=CARTESIAN_POINT('Ctrl Pts',(-13.0508216223155,41.1458333401613,-48.706329375));
#17234=CARTESIAN_POINT('Ctrl Pts',(1.59157945007855E-14,40.937500006828,
-48.706329375));
#17235=CARTESIAN_POINT('Ctrl Pts',(13.0508216223155,40.7291666734946,-48.706329375));
#17236=CARTESIAN_POINT('Ctrl Pts',(24.3531646875,40.5208333401613,-42.1809185638422));
#17237=CARTESIAN_POINT('Ctrl Pts',(35.6555077526845,40.312500006828,-35.6555077526845));
#17238=CARTESIAN_POINT('Ctrl Pts',(42.1809185638422,40.1041666734946,-24.3531646875));
#17239=CARTESIAN_POINT('Ctrl Pts',(48.706329375,39.8958333401613,-13.0508216223155));
#17240=CARTESIAN_POINT('Ctrl Pts',(48.706329375,39.687500006828,1.293339198242E-14));
#17241=CARTESIAN_POINT('Ctrl Pts',(48.706329375,39.4791666734946,13.0508216223155));
#17242=CARTESIAN_POINT('Ctrl Pts',(42.1809185638422,39.2708333401613,24.3531646875));
#17243=CARTESIAN_POINT('Ctrl Pts',(35.6555077526845,39.062500006828,35.6555077526845));
#17244=CARTESIAN_POINT('Ctrl Pts',(24.3531646875,38.8541666734946,42.1809185638422));
#17245=CARTESIAN_POINT('Ctrl Pts',(13.0508216223155,38.6458333401613,48.706329375));
#17246=CARTESIAN_POINT('Ctrl Pts',(-9.95098946405443E-15,38.437500006828,
48.706329375));
#17247=CARTESIAN_POINT('Ctrl Pts',(-13.0508216223155,38.2291666734946,48.706329375));
#17248=CARTESIAN_POINT('Ctrl Pts',(-24.3531646875,38.0208333401613,42.1809185638423));
#17249=CARTESIAN_POINT('Ctrl Pts',(-35.6555077526845,37.812500006828,35.6555077526845));
#17250=CARTESIAN_POINT('Ctrl Pts',(-42.1809185638422,37.6041666734946,24.3531646875));
#17251=CARTESIAN_POINT('Ctrl Pts',(-48.706329375,37.3958333401613,13.0508216223155));
#17252=CARTESIAN_POINT('Ctrl Pts',(-48.706329375,37.187500006828,-1.8898197019151E-14));
#17253=CARTESIAN_POINT('Ctrl Pts',(-48.706329375,36.9791666734946,-13.0508216223155));
#17254=CARTESIAN_POINT('Ctrl Pts',(-42.1809185638422,36.7708333401613,-24.3531646875));
#17255=CARTESIAN_POINT('Ctrl Pts',(-35.6555077526845,36.562500006828,-35.6555077526845));
#17256=CARTESIAN_POINT('Ctrl Pts',(-24.3531646875,36.3541666734946,-42.1809185638423));
#17257=CARTESIAN_POINT('Ctrl Pts',(-13.0508216223155,36.1458333401613,-48.706329375));
#17258=CARTESIAN_POINT('Ctrl Pts',(1.59157945007855E-14,35.937500006828,
-48.706329375));
#17259=CARTESIAN_POINT('Ctrl Pts',(13.0508216223155,35.7291666734946,-48.706329375));
#17260=CARTESIAN_POINT('Ctrl Pts',(24.3531646875,35.5208333401613,-42.1809185638422));
#17261=CARTESIAN_POINT('Ctrl Pts',(35.6555077526845,35.312500006828,-35.6555077526845));
#17262=CARTESIAN_POINT('Ctrl Pts',(42.1809185638422,35.1041666734946,-24.3531646875));
#17263=CARTESIAN_POINT('Ctrl Pts',(48.706329375,34.8958333401613,-13.0508216223155));
#17264=CARTESIAN_POINT('Ctrl Pts',(48.706329375,34.687500006828,1.293339198242E-14));
#17265=CARTESIAN_POINT('Ctrl Pts',(48.706329375,34.4791666734946,13.0508216223155));
#17266=CARTESIAN_POINT('Ctrl Pts',(42.1809185638422,34.2708333401613,24.3531646875));
#17267=CARTESIAN_POINT('Ctrl Pts',(35.6555077526845,34.062500006828,35.6555077526845));
#17268=CARTESIAN_POINT('Ctrl Pts',(24.3531646875,33.8541666734946,42.1809185638422));
#17269=CARTESIAN_POINT('Ctrl Pts',(13.0508216223155,33.6458333401613,48.706329375));
#17270=CARTESIAN_POINT('Ctrl Pts',(-9.95098946405443E-15,33.437500006828,
48.706329375));
#17271=CARTESIAN_POINT('Ctrl Pts',(-13.0508216223155,33.2291666734946,48.706329375));
#17272=CARTESIAN_POINT('Ctrl Pts',(-24.3531646875,33.0208333401613,42.1809185638423));
#17273=CARTESIAN_POINT('Ctrl Pts',(-35.6555077526845,32.812500006828,35.6555077526845));
#17274=CARTESIAN_POINT('Ctrl Pts',(-42.1809185638422,32.6041666734946,24.3531646875));
#17275=CARTESIAN_POINT('Ctrl Pts',(-48.706329375,32.3958333401613,13.0508216223155));
#17276=CARTESIAN_POINT('Ctrl Pts',(-48.706329375,32.187500006828,-1.8898197019151E-14));
#17277=CARTESIAN_POINT('Ctrl Pts',(-48.706329375,31.9791666734946,-13.0508216223155));
#17278=CARTESIAN_POINT('Ctrl Pts',(-42.1809185638422,31.7708333401613,-24.3531646875));
#17279=CARTESIAN_POINT('Ctrl Pts',(-35.6555077526845,31.562500006828,-35.6555077526845));
#17280=CARTESIAN_POINT('Ctrl Pts',(-24.3531646875,31.3541666734946,-42.1809185638423));
#17281=CARTESIAN_POINT('Ctrl Pts',(-13.0508216223155,31.1458333401613,-48.706329375));
#17282=CARTESIAN_POINT('Ctrl Pts',(1.59157945007855E-14,30.937500006828,
-48.706329375));
#17283=CARTESIAN_POINT('Ctrl Pts',(13.0508216223155,30.7291666734946,-48.706329375));
#17284=CARTESIAN_POINT('Ctrl Pts',(24.3531646875,30.5208333401613,-42.1809185638422));
#17285=CARTESIAN_POINT('Ctrl Pts',(35.6555077526845,30.312500006828,-35.6555077526845));
#17286=CARTESIAN_POINT('Ctrl Pts',(42.1809185638422,30.1041666734946,-24.3531646875));
#17287=CARTESIAN_POINT('Ctrl Pts',(48.706329375,29.8958333401613,-13.0508216223155));
#17288=CARTESIAN_POINT('Ctrl Pts',(48.706329375,29.687500006828,1.293339198242E-14));
#17289=CARTESIAN_POINT('Ctrl Pts',(48.706329375,29.4791666734946,13.0508216223155));
#17290=CARTESIAN_POINT('Ctrl Pts',(42.1809185638422,29.2708333401613,24.3531646875));
#17291=CARTESIAN_POINT('Ctrl Pts',(35.6555077526845,29.062500006828,35.6555077526845));
#17292=CARTESIAN_POINT('Ctrl Pts',(24.3531646875,28.8541666734946,42.1809185638422));
#17293=CARTESIAN_POINT('Ctrl Pts',(13.0508216223155,28.6458333401613,48.706329375));
#17294=CARTESIAN_POINT('Ctrl Pts',(-9.95098946405443E-15,28.437500006828,
48.706329375));
#17295=CARTESIAN_POINT('Ctrl Pts',(-13.0508216223155,28.2291666734946,48.706329375));
#17296=CARTESIAN_POINT('Ctrl Pts',(-24.3531646875,28.0208333401613,42.1809185638423));
#17297=CARTESIAN_POINT('Ctrl Pts',(-35.6555077526845,27.812500006828,35.6555077526845));
#17298=CARTESIAN_POINT('Ctrl Pts',(-42.1809185638422,27.6041666734946,24.3531646875));
#17299=CARTESIAN_POINT('Ctrl Pts',(-48.706329375,27.3958333401613,13.0508216223155));
#17300=CARTESIAN_POINT('Ctrl Pts',(-48.706329375,27.187500006828,-1.8898197019151E-14));
#17301=CARTESIAN_POINT('Origin',(-4513.80899805517,7988.28355096199,-4.33048917330144));
#17302=CARTESIAN_POINT('Ctrl Pts',(2.6308221862305,34.3301917962911,-45.9247076705387));
#17303=CARTESIAN_POINT('Ctrl Pts',(2.84524895812375,34.5752225485839,-46.3431776594255));
#17304=CARTESIAN_POINT('Ctrl Pts',(3.01791080422552,34.8332332645741,-46.7840354195864));
#17305=CARTESIAN_POINT('Ctrl Pts',(3.29117134372613,35.3512038226748,-47.6711182012495));
#17306=CARTESIAN_POINT('Ctrl Pts',(3.39456512521887,35.6166989155655,-48.1267924420204));
#17307=CARTESIAN_POINT('Ctrl Pts',(3.4681498498003,35.8816082987783,-48.5826971030357));
#17308=CARTESIAN_POINT('Ctrl Pts',(-46.,55.6250000136559,0.));
#17309=CARTESIAN_POINT('Ctrl Pts',(-46.,55.4166666803226,-12.3256628518316));
#17310=CARTESIAN_POINT('Ctrl Pts',(-39.8371685740842,55.2083333469893,-23.));
#17311=CARTESIAN_POINT('Ctrl Pts',(-33.6743371481684,55.0000000136559,-33.6743371481684));
#17312=CARTESIAN_POINT('Ctrl Pts',(-23.,54.7916666803226,-39.8371685740842));
#17313=CARTESIAN_POINT('Ctrl Pts',(-12.3256628518317,54.5833333469893,-46.));
#17314=CARTESIAN_POINT('Ctrl Pts',(-2.81668763803891E-15,54.3750000136559,
-46.));
#17315=CARTESIAN_POINT('Ctrl Pts',(12.3256628518316,54.1666666803226,-46.));
#17316=CARTESIAN_POINT('Ctrl Pts',(23.,53.9583333469893,-39.8371685740842));
#17317=CARTESIAN_POINT('Ctrl Pts',(33.6743371481683,53.7500000136559,-33.6743371481684));
#17318=CARTESIAN_POINT('Ctrl Pts',(39.8371685740842,53.5416666803226,-23.));
#17319=CARTESIAN_POINT('Ctrl Pts',(46.,53.3333333469893,-12.3256628518317));
#17320=CARTESIAN_POINT('Ctrl Pts',(46.,53.1250000136559,-5.63337527607782E-15));
#17321=CARTESIAN_POINT('Ctrl Pts',(46.,52.9166666803226,12.3256628518316));
#17322=CARTESIAN_POINT('Ctrl Pts',(39.8371685740842,52.7083333469893,23.));
#17323=CARTESIAN_POINT('Ctrl Pts',(33.6743371481684,52.5000000136559,33.6743371481683));
#17324=CARTESIAN_POINT('Ctrl Pts',(23.,52.2916666803226,39.8371685740842));
#17325=CARTESIAN_POINT('Ctrl Pts',(12.3256628518317,52.0833333469893,46.));
#17326=CARTESIAN_POINT('Ctrl Pts',(8.45006291411674E-15,51.8750000136559,
46.));
#17327=CARTESIAN_POINT('Ctrl Pts',(-12.3256628518316,51.6666666803226,46.));
#17328=CARTESIAN_POINT('Ctrl Pts',(-23.,51.4583333469893,39.8371685740842));
#17329=CARTESIAN_POINT('Ctrl Pts',(-33.6743371481683,51.2500000136559,33.6743371481684));
#17330=CARTESIAN_POINT('Ctrl Pts',(-39.8371685740842,51.0416666803226,23.));
#17331=CARTESIAN_POINT('Ctrl Pts',(-46.,50.8333333469893,12.3256628518317));
#17332=CARTESIAN_POINT('Ctrl Pts',(-46.,50.6250000136559,0.));
#17333=CARTESIAN_POINT('Ctrl Pts',(-46.,50.4166666803226,-12.3256628518316));
#17334=CARTESIAN_POINT('Ctrl Pts',(-39.8371685740842,50.2083333469893,-23.));
#17335=CARTESIAN_POINT('Ctrl Pts',(-33.6743371481684,50.0000000136559,-33.6743371481684));
#17336=CARTESIAN_POINT('Ctrl Pts',(-23.,49.7916666803226,-39.8371685740842));
#17337=CARTESIAN_POINT('Ctrl Pts',(-12.3256628518317,49.5833333469893,-46.));
#17338=CARTESIAN_POINT('Ctrl Pts',(-2.81668763803891E-15,49.3750000136559,
-46.));
#17339=CARTESIAN_POINT('Ctrl Pts',(12.3256628518316,49.1666666803226,-46.));
#17340=CARTESIAN_POINT('Ctrl Pts',(23.,48.9583333469893,-39.8371685740842));
#17341=CARTESIAN_POINT('Ctrl Pts',(33.6743371481683,48.7500000136559,-33.6743371481684));
#17342=CARTESIAN_POINT('Ctrl Pts',(39.8371685740842,48.5416666803226,-23.));
#17343=CARTESIAN_POINT('Ctrl Pts',(46.,48.3333333469893,-12.3256628518317));
#17344=CARTESIAN_POINT('Ctrl Pts',(46.,48.1250000136559,-5.63337527607782E-15));
#17345=CARTESIAN_POINT('Ctrl Pts',(46.,47.9166666803226,12.3256628518316));
#17346=CARTESIAN_POINT('Ctrl Pts',(39.8371685740842,47.7083333469893,23.));
#17347=CARTESIAN_POINT('Ctrl Pts',(33.6743371481684,47.5000000136559,33.6743371481683));
#17348=CARTESIAN_POINT('Ctrl Pts',(23.,47.2916666803226,39.8371685740842));
#17349=CARTESIAN_POINT('Ctrl Pts',(12.3256628518317,47.0833333469893,46.));
#17350=CARTESIAN_POINT('Ctrl Pts',(8.45006291411674E-15,46.8750000136559,
46.));
#17351=CARTESIAN_POINT('Ctrl Pts',(-12.3256628518316,46.6666666803226,46.));
#17352=CARTESIAN_POINT('Ctrl Pts',(-23.,46.4583333469893,39.8371685740842));
#17353=CARTESIAN_POINT('Ctrl Pts',(-33.6743371481683,46.2500000136559,33.6743371481684));
#17354=CARTESIAN_POINT('Ctrl Pts',(-39.8371685740842,46.0416666803226,23.));
#17355=CARTESIAN_POINT('Ctrl Pts',(-46.,45.8333333469892,12.3256628518317));
#17356=CARTESIAN_POINT('Ctrl Pts',(-46.,45.6250000136559,0.));
#17357=CARTESIAN_POINT('Ctrl Pts',(-46.,45.4166666803226,-12.3256628518316));
#17358=CARTESIAN_POINT('Ctrl Pts',(-39.8371685740842,45.2083333469893,-23.));
#17359=CARTESIAN_POINT('Ctrl Pts',(-33.6743371481684,45.0000000136559,-33.6743371481684));
#17360=CARTESIAN_POINT('Ctrl Pts',(-23.,44.7916666803226,-39.8371685740842));
#17361=CARTESIAN_POINT('Ctrl Pts',(-12.3256628518317,44.5833333469893,-46.));
#17362=CARTESIAN_POINT('Ctrl Pts',(-2.81668763803891E-15,44.3750000136559,
-46.));
#17363=CARTESIAN_POINT('Ctrl Pts',(12.3256628518316,44.1666666803226,-46.));
#17364=CARTESIAN_POINT('Ctrl Pts',(23.,43.9583333469893,-39.8371685740842));
#17365=CARTESIAN_POINT('Ctrl Pts',(33.6743371481683,43.7500000136559,-33.6743371481684));
#17366=CARTESIAN_POINT('Ctrl Pts',(39.8371685740842,43.5416666803226,-23.));
#17367=CARTESIAN_POINT('Ctrl Pts',(46.,43.3333333469893,-12.3256628518317));
#17368=CARTESIAN_POINT('Ctrl Pts',(46.,43.1250000136559,-5.63337527607782E-15));
#17369=CARTESIAN_POINT('Ctrl Pts',(46.,42.9166666803226,12.3256628518316));
#17370=CARTESIAN_POINT('Ctrl Pts',(39.8371685740842,42.7083333469893,23.));
#17371=CARTESIAN_POINT('Ctrl Pts',(33.6743371481684,42.5000000136559,33.6743371481683));
#17372=CARTESIAN_POINT('Ctrl Pts',(23.,42.2916666803226,39.8371685740842));
#17373=CARTESIAN_POINT('Ctrl Pts',(12.3256628518317,42.0833333469893,46.));
#17374=CARTESIAN_POINT('Ctrl Pts',(8.45006291411674E-15,41.8750000136559,
46.));
#17375=CARTESIAN_POINT('Ctrl Pts',(-12.3256628518316,41.6666666803226,46.));
#17376=CARTESIAN_POINT('Ctrl Pts',(-23.,41.4583333469893,39.8371685740842));
#17377=CARTESIAN_POINT('Ctrl Pts',(-33.6743371481683,41.2500000136559,33.6743371481684));
#17378=CARTESIAN_POINT('Ctrl Pts',(-39.8371685740842,41.0416666803226,23.));
#17379=CARTESIAN_POINT('Ctrl Pts',(-46.,40.8333333469893,12.3256628518317));
#17380=CARTESIAN_POINT('Ctrl Pts',(-46.,40.6250000136559,0.));
#17381=CARTESIAN_POINT('Ctrl Pts',(-46.,40.4166666803226,-12.3256628518316));
#17382=CARTESIAN_POINT('Ctrl Pts',(-39.8371685740842,40.2083333469893,-23.));
#17383=CARTESIAN_POINT('Ctrl Pts',(-33.6743371481684,40.0000000136559,-33.6743371481684));
#17384=CARTESIAN_POINT('Ctrl Pts',(-23.,39.7916666803226,-39.8371685740842));
#17385=CARTESIAN_POINT('Ctrl Pts',(-12.3256628518317,39.5833333469893,-46.));
#17386=CARTESIAN_POINT('Ctrl Pts',(-2.81668763803891E-15,39.3750000136559,
-46.));
#17387=CARTESIAN_POINT('Ctrl Pts',(12.3256628518316,39.1666666803226,-46.));
#17388=CARTESIAN_POINT('Ctrl Pts',(23.,38.9583333469893,-39.8371685740842));
#17389=CARTESIAN_POINT('Ctrl Pts',(33.6743371481683,38.7500000136559,-33.6743371481684));
#17390=CARTESIAN_POINT('Ctrl Pts',(39.8371685740842,38.5416666803226,-23.));
#17391=CARTESIAN_POINT('Ctrl Pts',(46.,38.3333333469893,-12.3256628518317));
#17392=CARTESIAN_POINT('Ctrl Pts',(46.,38.1250000136559,-5.63337527607782E-15));
#17393=CARTESIAN_POINT('Ctrl Pts',(46.,37.9166666803226,12.3256628518316));
#17394=CARTESIAN_POINT('Ctrl Pts',(39.8371685740842,37.7083333469893,23.));
#17395=CARTESIAN_POINT('Ctrl Pts',(33.6743371481684,37.5000000136559,33.6743371481683));
#17396=CARTESIAN_POINT('Ctrl Pts',(23.,37.2916666803226,39.8371685740842));
#17397=CARTESIAN_POINT('Ctrl Pts',(12.3256628518317,37.0833333469893,46.));
#17398=CARTESIAN_POINT('Ctrl Pts',(8.45006291411674E-15,36.8750000136559,
46.));
#17399=CARTESIAN_POINT('Ctrl Pts',(-12.3256628518316,36.6666666803226,46.));
#17400=CARTESIAN_POINT('Ctrl Pts',(-23.,36.4583333469893,39.8371685740842));
#17401=CARTESIAN_POINT('Ctrl Pts',(-33.6743371481683,36.2500000136559,33.6743371481684));
#17402=CARTESIAN_POINT('Ctrl Pts',(-39.8371685740842,36.0416666803226,23.));
#17403=CARTESIAN_POINT('Ctrl Pts',(-46.,35.8333333469893,12.3256628518317));
#17404=CARTESIAN_POINT('Ctrl Pts',(-46.,35.6250000136559,0.));
#17405=CARTESIAN_POINT('Ctrl Pts',(-46.,35.4166666803226,-12.3256628518316));
#17406=CARTESIAN_POINT('Ctrl Pts',(-39.8371685740842,35.2083333469893,-23.));
#17407=CARTESIAN_POINT('Ctrl Pts',(-33.6743371481684,35.0000000136559,-33.6743371481684));
#17408=CARTESIAN_POINT('Ctrl Pts',(-23.,34.7916666803226,-39.8371685740842));
#17409=CARTESIAN_POINT('Ctrl Pts',(-12.3256628518317,34.5833333469893,-46.));
#17410=CARTESIAN_POINT('Ctrl Pts',(-2.81668763803891E-15,34.3750000136559,
-46.));
#17411=CARTESIAN_POINT('Ctrl Pts',(12.3256628518316,34.1666666803226,-46.));
#17412=CARTESIAN_POINT('Ctrl Pts',(23.,33.9583333469893,-39.8371685740842));
#17413=CARTESIAN_POINT('Ctrl Pts',(33.6743371481683,33.7500000136559,-33.6743371481684));
#17414=CARTESIAN_POINT('Ctrl Pts',(39.8371685740842,33.5416666803226,-23.));
#17415=CARTESIAN_POINT('Ctrl Pts',(46.,33.3333333469893,-12.3256628518317));
#17416=CARTESIAN_POINT('Ctrl Pts',(46.,33.1250000136559,-5.63337527607782E-15));
#17417=CARTESIAN_POINT('Ctrl Pts',(46.,32.9166666803226,12.3256628518316));
#17418=CARTESIAN_POINT('Ctrl Pts',(39.8371685740842,32.7083333469893,23.));
#17419=CARTESIAN_POINT('Ctrl Pts',(33.6743371481684,32.5000000136559,33.6743371481683));
#17420=CARTESIAN_POINT('Ctrl Pts',(23.,32.2916666803226,39.8371685740842));
#17421=CARTESIAN_POINT('Ctrl Pts',(12.3256628518317,32.0833333469893,46.));
#17422=CARTESIAN_POINT('Ctrl Pts',(8.45006291411674E-15,31.8750000136559,
46.));
#17423=CARTESIAN_POINT('Ctrl Pts',(-12.3256628518316,31.6666666803226,46.));
#17424=CARTESIAN_POINT('Ctrl Pts',(-23.,31.4583333469893,39.8371685740842));
#17425=CARTESIAN_POINT('Ctrl Pts',(-33.6743371481683,31.2500000136559,33.6743371481684));
#17426=CARTESIAN_POINT('Ctrl Pts',(-39.8371685740842,31.0416666803226,23.));
#17427=CARTESIAN_POINT('Ctrl Pts',(-46.,30.8333333469893,12.3256628518317));
#17428=CARTESIAN_POINT('Ctrl Pts',(-46.,30.6250000136559,0.));
#17429=CARTESIAN_POINT('Ctrl Pts',(-46.,30.4166666803226,-12.3256628518316));
#17430=CARTESIAN_POINT('Ctrl Pts',(-39.8371685740842,30.2083333469893,-23.));
#17431=CARTESIAN_POINT('Ctrl Pts',(-33.6743371481684,30.0000000136559,-33.6743371481684));
#17432=CARTESIAN_POINT('Ctrl Pts',(-23.,29.7916666803226,-39.8371685740842));
#17433=CARTESIAN_POINT('Ctrl Pts',(-12.3256628518317,29.5833333469893,-46.));
#17434=CARTESIAN_POINT('Ctrl Pts',(-2.81668763803891E-15,29.3750000136559,
-46.));
#17435=CARTESIAN_POINT('Ctrl Pts',(12.3256628518316,29.1666666803226,-46.));
#17436=CARTESIAN_POINT('Ctrl Pts',(23.,28.9583333469893,-39.8371685740842));
#17437=CARTESIAN_POINT('Ctrl Pts',(33.6743371481683,28.7500000136559,-33.6743371481684));
#17438=CARTESIAN_POINT('Ctrl Pts',(39.8371685740842,28.5416666803226,-23.));
#17439=CARTESIAN_POINT('Ctrl Pts',(46.,28.3333333469893,-12.3256628518317));
#17440=CARTESIAN_POINT('Ctrl Pts',(46.,28.1250000136559,-5.63337527607782E-15));
#17441=CARTESIAN_POINT('Ctrl Pts',(46.,27.9166666803226,12.3256628518316));
#17442=CARTESIAN_POINT('Ctrl Pts',(39.8371685740842,27.7083333469893,23.));
#17443=CARTESIAN_POINT('Ctrl Pts',(33.6743371481684,27.5000000136559,33.6743371481683));
#17444=CARTESIAN_POINT('Ctrl Pts',(23.,27.2916666803226,39.8371685740842));
#17445=CARTESIAN_POINT('Ctrl Pts',(12.3256628518317,27.0833333469893,46.));
#17446=CARTESIAN_POINT('Ctrl Pts',(8.45006291411674E-15,26.8750000136559,
46.));
#17447=CARTESIAN_POINT('Ctrl Pts',(-12.3256628518316,26.6666666803226,46.));
#17448=CARTESIAN_POINT('Ctrl Pts',(-23.,26.4583333469893,39.8371685740842));
#17449=CARTESIAN_POINT('Ctrl Pts',(-33.6743371481683,26.2500000136559,33.6743371481684));
#17450=CARTESIAN_POINT('Ctrl Pts',(-39.8371685740842,26.0416666803226,23.));
#17451=CARTESIAN_POINT('Ctrl Pts',(-46.,25.8333333469893,12.3256628518317));
#17452=CARTESIAN_POINT('Ctrl Pts',(-46.,25.6250000136559,0.));
#17453=CARTESIAN_POINT('Ctrl Pts',(-48.706329375,57.187500006828,-1.8898197019151E-14));
#17454=CARTESIAN_POINT('Ctrl Pts',(-48.706329375,56.9791666734946,-13.0508216223155));
#17455=CARTESIAN_POINT('Ctrl Pts',(-42.1809185638422,56.7708333401613,-24.3531646875));
#17456=CARTESIAN_POINT('Ctrl Pts',(-35.6555077526845,56.562500006828,-35.6555077526845));
#17457=CARTESIAN_POINT('Ctrl Pts',(-24.3531646875,56.3541666734946,-42.1809185638423));
#17458=CARTESIAN_POINT('Ctrl Pts',(-13.0508216223155,56.1458333401613,-48.706329375));
#17459=CARTESIAN_POINT('Ctrl Pts',(1.59157945007855E-14,55.937500006828,
-48.706329375));
#17460=CARTESIAN_POINT('Ctrl Pts',(13.0508216223155,55.7291666734946,-48.706329375));
#17461=CARTESIAN_POINT('Ctrl Pts',(24.3531646875,55.5208333401613,-42.1809185638422));
#17462=CARTESIAN_POINT('Ctrl Pts',(35.6555077526845,55.312500006828,-35.6555077526845));
#17463=CARTESIAN_POINT('Ctrl Pts',(42.1809185638422,55.1041666734946,-24.3531646875));
#17464=CARTESIAN_POINT('Ctrl Pts',(48.706329375,54.8958333401613,-13.0508216223155));
#17465=CARTESIAN_POINT('Ctrl Pts',(48.706329375,54.687500006828,1.293339198242E-14));
#17466=CARTESIAN_POINT('Ctrl Pts',(48.706329375,54.4791666734946,13.0508216223155));
#17467=CARTESIAN_POINT('Ctrl Pts',(42.1809185638422,54.2708333401613,24.3531646875));
#17468=CARTESIAN_POINT('Ctrl Pts',(35.6555077526845,54.062500006828,35.6555077526845));
#17469=CARTESIAN_POINT('Ctrl Pts',(24.3531646875,53.8541666734946,42.1809185638422));
#17470=CARTESIAN_POINT('Ctrl Pts',(13.0508216223155,53.6458333401613,48.706329375));
#17471=CARTESIAN_POINT('Ctrl Pts',(-9.95098946405443E-15,53.437500006828,
48.706329375));
#17472=CARTESIAN_POINT('Ctrl Pts',(-13.0508216223155,53.2291666734946,48.706329375));
#17473=CARTESIAN_POINT('Ctrl Pts',(-24.3531646875,53.0208333401613,42.1809185638423));
#17474=CARTESIAN_POINT('Ctrl Pts',(-35.6555077526845,52.812500006828,35.6555077526845));
#17475=CARTESIAN_POINT('Ctrl Pts',(-42.1809185638422,52.6041666734946,24.3531646875));
#17476=CARTESIAN_POINT('Ctrl Pts',(-48.706329375,52.3958333401613,13.0508216223155));
#17477=CARTESIAN_POINT('Ctrl Pts',(-48.706329375,52.187500006828,-1.8898197019151E-14));
#17478=CARTESIAN_POINT('Ctrl Pts',(-48.706329375,51.9791666734946,-13.0508216223155));
#17479=CARTESIAN_POINT('Ctrl Pts',(-42.1809185638422,51.7708333401613,-24.3531646875));
#17480=CARTESIAN_POINT('Ctrl Pts',(-35.6555077526845,51.562500006828,-35.6555077526845));
#17481=CARTESIAN_POINT('Ctrl Pts',(-24.3531646875,51.3541666734946,-42.1809185638423));
#17482=CARTESIAN_POINT('Ctrl Pts',(-13.0508216223155,51.1458333401613,-48.706329375));
#17483=CARTESIAN_POINT('Ctrl Pts',(1.59157945007855E-14,50.937500006828,
-48.706329375));
#17484=CARTESIAN_POINT('Ctrl Pts',(13.0508216223155,50.7291666734946,-48.706329375));
#17485=CARTESIAN_POINT('Ctrl Pts',(24.3531646875,50.5208333401613,-42.1809185638422));
#17486=CARTESIAN_POINT('Ctrl Pts',(35.6555077526845,50.312500006828,-35.6555077526845));
#17487=CARTESIAN_POINT('Ctrl Pts',(42.1809185638422,50.1041666734946,-24.3531646875));
#17488=CARTESIAN_POINT('Ctrl Pts',(48.706329375,49.8958333401613,-13.0508216223155));
#17489=CARTESIAN_POINT('Ctrl Pts',(48.706329375,49.687500006828,1.293339198242E-14));
#17490=CARTESIAN_POINT('Ctrl Pts',(48.706329375,49.4791666734946,13.0508216223155));
#17491=CARTESIAN_POINT('Ctrl Pts',(42.1809185638422,49.2708333401613,24.3531646875));
#17492=CARTESIAN_POINT('Ctrl Pts',(35.6555077526845,49.062500006828,35.6555077526845));
#17493=CARTESIAN_POINT('Ctrl Pts',(24.3531646875,48.8541666734946,42.1809185638422));
#17494=CARTESIAN_POINT('Ctrl Pts',(13.0508216223155,48.6458333401613,48.706329375));
#17495=CARTESIAN_POINT('Ctrl Pts',(-9.95098946405443E-15,48.437500006828,
48.706329375));
#17496=CARTESIAN_POINT('Ctrl Pts',(-13.0508216223155,48.2291666734946,48.706329375));
#17497=CARTESIAN_POINT('Ctrl Pts',(-24.3531646875,48.0208333401613,42.1809185638423));
#17498=CARTESIAN_POINT('Ctrl Pts',(-35.6555077526845,47.812500006828,35.6555077526845));
#17499=CARTESIAN_POINT('Ctrl Pts',(-42.1809185638422,47.6041666734946,24.3531646875));
#17500=CARTESIAN_POINT('Ctrl Pts',(-48.706329375,47.3958333401613,13.0508216223155));
#17501=CARTESIAN_POINT('Ctrl Pts',(-48.706329375,47.187500006828,-1.8898197019151E-14));
#17502=CARTESIAN_POINT('Ctrl Pts',(-48.706329375,46.9791666734946,-13.0508216223155));
#17503=CARTESIAN_POINT('Ctrl Pts',(-42.1809185638422,46.7708333401613,-24.3531646875));
#17504=CARTESIAN_POINT('Ctrl Pts',(-35.6555077526845,46.562500006828,-35.6555077526845));
#17505=CARTESIAN_POINT('Ctrl Pts',(-24.3531646875,46.3541666734946,-42.1809185638423));
#17506=CARTESIAN_POINT('Ctrl Pts',(-13.0508216223155,46.1458333401613,-48.706329375));
#17507=CARTESIAN_POINT('Ctrl Pts',(1.59157945007855E-14,45.937500006828,
-48.706329375));
#17508=CARTESIAN_POINT('Ctrl Pts',(13.0508216223155,45.7291666734946,-48.706329375));
#17509=CARTESIAN_POINT('Ctrl Pts',(24.3531646875,45.5208333401613,-42.1809185638422));
#17510=CARTESIAN_POINT('Ctrl Pts',(35.6555077526845,45.312500006828,-35.6555077526845));
#17511=CARTESIAN_POINT('Ctrl Pts',(42.1809185638422,45.1041666734946,-24.3531646875));
#17512=CARTESIAN_POINT('Ctrl Pts',(48.706329375,44.8958333401613,-13.0508216223155));
#17513=CARTESIAN_POINT('Ctrl Pts',(48.706329375,44.687500006828,1.293339198242E-14));
#17514=CARTESIAN_POINT('Ctrl Pts',(48.706329375,44.4791666734946,13.0508216223155));
#17515=CARTESIAN_POINT('Ctrl Pts',(42.1809185638422,44.2708333401613,24.3531646875));
#17516=CARTESIAN_POINT('Ctrl Pts',(35.6555077526845,44.062500006828,35.6555077526845));
#17517=CARTESIAN_POINT('Ctrl Pts',(24.3531646875,43.8541666734946,42.1809185638422));
#17518=CARTESIAN_POINT('Ctrl Pts',(13.0508216223155,43.6458333401613,48.706329375));
#17519=CARTESIAN_POINT('Ctrl Pts',(-9.95098946405443E-15,43.437500006828,
48.706329375));
#17520=CARTESIAN_POINT('Ctrl Pts',(-13.0508216223155,43.2291666734946,48.706329375));
#17521=CARTESIAN_POINT('Ctrl Pts',(-24.3531646875,43.0208333401613,42.1809185638423));
#17522=CARTESIAN_POINT('Ctrl Pts',(-35.6555077526845,42.812500006828,35.6555077526845));
#17523=CARTESIAN_POINT('Ctrl Pts',(-42.1809185638422,42.6041666734946,24.3531646875));
#17524=CARTESIAN_POINT('Ctrl Pts',(-48.706329375,42.3958333401613,13.0508216223155));
#17525=CARTESIAN_POINT('Ctrl Pts',(-48.706329375,42.187500006828,-1.8898197019151E-14));
#17526=CARTESIAN_POINT('Ctrl Pts',(-48.706329375,41.9791666734946,-13.0508216223155));
#17527=CARTESIAN_POINT('Ctrl Pts',(-42.1809185638422,41.7708333401613,-24.3531646875));
#17528=CARTESIAN_POINT('Ctrl Pts',(-35.6555077526845,41.562500006828,-35.6555077526845));
#17529=CARTESIAN_POINT('Ctrl Pts',(-24.3531646875,41.3541666734946,-42.1809185638423));
#17530=CARTESIAN_POINT('Ctrl Pts',(-13.0508216223155,41.1458333401613,-48.706329375));
#17531=CARTESIAN_POINT('Ctrl Pts',(1.59157945007855E-14,40.937500006828,
-48.706329375));
#17532=CARTESIAN_POINT('Ctrl Pts',(13.0508216223155,40.7291666734946,-48.706329375));
#17533=CARTESIAN_POINT('Ctrl Pts',(24.3531646875,40.5208333401613,-42.1809185638422));
#17534=CARTESIAN_POINT('Ctrl Pts',(35.6555077526845,40.312500006828,-35.6555077526845));
#17535=CARTESIAN_POINT('Ctrl Pts',(42.1809185638422,40.1041666734946,-24.3531646875));
#17536=CARTESIAN_POINT('Ctrl Pts',(48.706329375,39.8958333401613,-13.0508216223155));
#17537=CARTESIAN_POINT('Ctrl Pts',(48.706329375,39.687500006828,1.293339198242E-14));
#17538=CARTESIAN_POINT('Ctrl Pts',(48.706329375,39.4791666734946,13.0508216223155));
#17539=CARTESIAN_POINT('Ctrl Pts',(42.1809185638422,39.2708333401613,24.3531646875));
#17540=CARTESIAN_POINT('Ctrl Pts',(35.6555077526845,39.062500006828,35.6555077526845));
#17541=CARTESIAN_POINT('Ctrl Pts',(24.3531646875,38.8541666734946,42.1809185638422));
#17542=CARTESIAN_POINT('Ctrl Pts',(13.0508216223155,38.6458333401613,48.706329375));
#17543=CARTESIAN_POINT('Ctrl Pts',(-9.95098946405443E-15,38.437500006828,
48.706329375));
#17544=CARTESIAN_POINT('Ctrl Pts',(-13.0508216223155,38.2291666734946,48.706329375));
#17545=CARTESIAN_POINT('Ctrl Pts',(-24.3531646875,38.0208333401613,42.1809185638423));
#17546=CARTESIAN_POINT('Ctrl Pts',(-35.6555077526845,37.812500006828,35.6555077526845));
#17547=CARTESIAN_POINT('Ctrl Pts',(-42.1809185638422,37.6041666734946,24.3531646875));
#17548=CARTESIAN_POINT('Ctrl Pts',(-48.706329375,37.3958333401613,13.0508216223155));
#17549=CARTESIAN_POINT('Ctrl Pts',(-48.706329375,37.187500006828,-1.8898197019151E-14));
#17550=CARTESIAN_POINT('Ctrl Pts',(-48.706329375,36.9791666734946,-13.0508216223155));
#17551=CARTESIAN_POINT('Ctrl Pts',(-42.1809185638422,36.7708333401613,-24.3531646875));
#17552=CARTESIAN_POINT('Ctrl Pts',(-35.6555077526845,36.562500006828,-35.6555077526845));
#17553=CARTESIAN_POINT('Ctrl Pts',(-24.3531646875,36.3541666734946,-42.1809185638423));
#17554=CARTESIAN_POINT('Ctrl Pts',(-13.0508216223155,36.1458333401613,-48.706329375));
#17555=CARTESIAN_POINT('Ctrl Pts',(1.59157945007855E-14,35.937500006828,
-48.706329375));
#17556=CARTESIAN_POINT('Ctrl Pts',(13.0508216223155,35.7291666734946,-48.706329375));
#17557=CARTESIAN_POINT('Ctrl Pts',(24.3531646875,35.5208333401613,-42.1809185638422));
#17558=CARTESIAN_POINT('Ctrl Pts',(35.6555077526845,35.312500006828,-35.6555077526845));
#17559=CARTESIAN_POINT('Ctrl Pts',(42.1809185638422,35.1041666734946,-24.3531646875));
#17560=CARTESIAN_POINT('Ctrl Pts',(48.706329375,34.8958333401613,-13.0508216223155));
#17561=CARTESIAN_POINT('Ctrl Pts',(48.706329375,34.687500006828,1.293339198242E-14));
#17562=CARTESIAN_POINT('Ctrl Pts',(48.706329375,34.4791666734946,13.0508216223155));
#17563=CARTESIAN_POINT('Ctrl Pts',(42.1809185638422,34.2708333401613,24.3531646875));
#17564=CARTESIAN_POINT('Ctrl Pts',(35.6555077526845,34.062500006828,35.6555077526845));
#17565=CARTESIAN_POINT('Ctrl Pts',(24.3531646875,33.8541666734946,42.1809185638422));
#17566=CARTESIAN_POINT('Ctrl Pts',(13.0508216223155,33.6458333401613,48.706329375));
#17567=CARTESIAN_POINT('Ctrl Pts',(-9.95098946405443E-15,33.437500006828,
48.706329375));
#17568=CARTESIAN_POINT('Ctrl Pts',(-13.0508216223155,33.2291666734946,48.706329375));
#17569=CARTESIAN_POINT('Ctrl Pts',(-24.3531646875,33.0208333401613,42.1809185638423));
#17570=CARTESIAN_POINT('Ctrl Pts',(-35.6555077526845,32.812500006828,35.6555077526845));
#17571=CARTESIAN_POINT('Ctrl Pts',(-42.1809185638422,32.6041666734946,24.3531646875));
#17572=CARTESIAN_POINT('Ctrl Pts',(-48.706329375,32.3958333401613,13.0508216223155));
#17573=CARTESIAN_POINT('Ctrl Pts',(-48.706329375,32.187500006828,-1.8898197019151E-14));
#17574=CARTESIAN_POINT('Ctrl Pts',(-48.706329375,31.9791666734946,-13.0508216223155));
#17575=CARTESIAN_POINT('Ctrl Pts',(-42.1809185638422,31.7708333401613,-24.3531646875));
#17576=CARTESIAN_POINT('Ctrl Pts',(-35.6555077526845,31.562500006828,-35.6555077526845));
#17577=CARTESIAN_POINT('Ctrl Pts',(-24.3531646875,31.3541666734946,-42.1809185638423));
#17578=CARTESIAN_POINT('Ctrl Pts',(-13.0508216223155,31.1458333401613,-48.706329375));
#17579=CARTESIAN_POINT('Ctrl Pts',(1.59157945007855E-14,30.937500006828,
-48.706329375));
#17580=CARTESIAN_POINT('Ctrl Pts',(13.0508216223155,30.7291666734946,-48.706329375));
#17581=CARTESIAN_POINT('Ctrl Pts',(24.3531646875,30.5208333401613,-42.1809185638422));
#17582=CARTESIAN_POINT('Ctrl Pts',(35.6555077526845,30.312500006828,-35.6555077526845));
#17583=CARTESIAN_POINT('Ctrl Pts',(42.1809185638422,30.1041666734946,-24.3531646875));
#17584=CARTESIAN_POINT('Ctrl Pts',(48.706329375,29.8958333401613,-13.0508216223155));
#17585=CARTESIAN_POINT('Ctrl Pts',(48.706329375,29.687500006828,1.293339198242E-14));
#17586=CARTESIAN_POINT('Ctrl Pts',(48.706329375,29.4791666734946,13.0508216223155));
#17587=CARTESIAN_POINT('Ctrl Pts',(42.1809185638422,29.2708333401613,24.3531646875));
#17588=CARTESIAN_POINT('Ctrl Pts',(35.6555077526845,29.062500006828,35.6555077526845));
#17589=CARTESIAN_POINT('Ctrl Pts',(24.3531646875,28.8541666734946,42.1809185638422));
#17590=CARTESIAN_POINT('Ctrl Pts',(13.0508216223155,28.6458333401613,48.706329375));
#17591=CARTESIAN_POINT('Ctrl Pts',(-9.95098946405443E-15,28.437500006828,
48.706329375));
#17592=CARTESIAN_POINT('Ctrl Pts',(-13.0508216223155,28.2291666734946,48.706329375));
#17593=CARTESIAN_POINT('Ctrl Pts',(-24.3531646875,28.0208333401613,42.1809185638423));
#17594=CARTESIAN_POINT('Ctrl Pts',(-35.6555077526845,27.812500006828,35.6555077526845));
#17595=CARTESIAN_POINT('Ctrl Pts',(-42.1809185638422,27.6041666734946,24.3531646875));
#17596=CARTESIAN_POINT('Ctrl Pts',(-48.706329375,27.3958333401613,13.0508216223155));
#17597=CARTESIAN_POINT('Ctrl Pts',(-48.706329375,27.187500006828,-1.8898197019151E-14));
#17598=CARTESIAN_POINT('',(-2.14849279754675,33.4030003256338,48.658920044375));
#17599=CARTESIAN_POINT('',(-48.5725845633798,32.2456516907297,3.60701400320324));
#17600=CARTESIAN_POINT('Ctrl Pts',(-2.14849279754675,33.4030003256338,48.658920044375));
#17601=CARTESIAN_POINT('Ctrl Pts',(-14.0425623011786,33.2108861594244,48.1337476270921));
#17602=CARTESIAN_POINT('Ctrl Pts',(-24.3531646875,33.0208333401613,42.1809185638423));
#17603=CARTESIAN_POINT('Ctrl Pts',(-35.6555077526845,32.812500006828,35.6555077526845));
#17604=CARTESIAN_POINT('Ctrl Pts',(-42.1809185638422,32.6041666734946,24.3531646875));
#17605=CARTESIAN_POINT('Ctrl Pts',(-47.7480251419552,32.4264286116308,14.7106532430575));
#17606=CARTESIAN_POINT('Ctrl Pts',(-48.5725845633798,32.2456516907297,3.60701400320324));
#17607=CARTESIAN_POINT('Ctrl Pts',(-48.5725845633798,32.2456516907297,3.60701400320324));
#17608=CARTESIAN_POINT('Ctrl Pts',(-48.3407853679392,32.1124685639422,3.60701400320324));
#17609=CARTESIAN_POINT('Ctrl Pts',(-48.1089821836664,31.9792923792741,3.60701400320324));
#17610=CARTESIAN_POINT('Ctrl Pts',(-47.6453674864979,31.7129545080418,3.60701400320324));
#17611=CARTESIAN_POINT('Ctrl Pts',(-47.4135559734253,31.5797928212585,3.60701400320323));
#17612=CARTESIAN_POINT('Ctrl Pts',(-47.1817401099609,31.4466387085919,3.60701400320323));
#17613=CARTESIAN_POINT('Ctrl Pts',(-46.7406305897488,31.1932671494809,3.60701400320323));
#17614=CARTESIAN_POINT('Ctrl Pts',(-46.2995053259033,30.9399229970588,3.60701400320325));
#17615=CARTESIAN_POINT('Ctrl Pts',(-45.858362923034,30.686608693912,3.60701400320327));
#17616=CARTESIAN_POINT('Ctrl Pts',(45.858362923034,33.0633913333999,3.60701400320327));
#17617=CARTESIAN_POINT('Ctrl Pts',(46.0899257719339,33.1969849680263,3.60701400320326));
#17618=CARTESIAN_POINT('Ctrl Pts',(46.5530501979845,33.4641744416604,3.60701400320347));
#17619=CARTESIAN_POINT('Ctrl Pts',(47.0161721905706,33.7313681332063,3.60701400320335));
#17620=CARTESIAN_POINT('Ctrl Pts',(47.6893519862319,34.1197565257476,3.60701400320335));
#17621=CARTESIAN_POINT('Ctrl Pts',(48.1309692507095,34.3745507329179,3.60701400320329));
#17622=CARTESIAN_POINT('Ctrl Pts',(48.5725845633798,34.6293483229262,3.60701400320329));
#17623=CARTESIAN_POINT('Ctrl Pts',(1.54954344745633,33.4623411901214,48.6816745427932));
#17624=CARTESIAN_POINT('Ctrl Pts',(1.37917007070576,33.3690980212298,48.5301278551423));
#17625=CARTESIAN_POINT('Ctrl Pts',(1.19203308366643,33.282927635968,48.3910568573769));
#17626=CARTESIAN_POINT('Ctrl Pts',(0.805625630179277,33.1438388130886,48.1687150028693));
#17627=CARTESIAN_POINT('Ctrl Pts',(0.609847947224847,33.0885120549907,48.08133053428));
#17628=CARTESIAN_POINT('Ctrl Pts',(0.260777891394813,33.0206023207758,47.9764123934958));
#17629=CARTESIAN_POINT('Ctrl Pts',(0.115525945788527,33.0003237004996,47.9459618456904));
#17630=CARTESIAN_POINT('Ctrl Pts',(-0.115776397631957,32.9814498550727,
47.9196126328073));
#17631=CARTESIAN_POINT('Ctrl Pts',(-0.198964591777061,32.9772746441304,
47.9144499859977));
#17632=CARTESIAN_POINT('Ctrl Pts',(-0.284246351598831,32.9756985844503,
47.9136181470705));
#17633=CARTESIAN_POINT('Ctrl Pts',(-0.28600879736358,32.9756671879154,47.9136028937503));
#17634=CARTESIAN_POINT('Ctrl Pts',(-0.288399652950703,32.9756261901408,
47.9135848302284));
#17635=CARTESIAN_POINT('Ctrl Pts',(-0.289028030011347,32.9756155641944,
47.9135803289705));
#17636=CARTESIAN_POINT('Ctrl Pts',(-0.290151105636925,32.9755968396661,
47.9135727242207));
#17637=CARTESIAN_POINT('Ctrl Pts',(-0.290645802456765,32.9755886843435,
47.9135695270925));
#17638=CARTESIAN_POINT('Ctrl Pts',(-0.291615609203089,32.9755728779986,
47.9135635586627));
#17639=CARTESIAN_POINT('Ctrl Pts',(-0.292090718753741,32.9755652197985,
47.9135607755125));
#17640=CARTESIAN_POINT('Ctrl Pts',(-0.29321670374883,32.9755472725322,47.9135545132575));
#17641=CARTESIAN_POINT('Ctrl Pts',(-0.293867580950652,32.9755370582652,
47.9135511575783));
#17642=CARTESIAN_POINT('Ctrl Pts',(-0.296001919607553,32.9755040891644,
47.9135410201668));
#17643=CARTESIAN_POINT('Ctrl Pts',(-0.297485395190452,32.975482005975,47.9135353466702));
#17644=CARTESIAN_POINT('Ctrl Pts',(-0.341549846483652,32.9748507718471,
47.9134075922713));
#17645=CARTESIAN_POINT('Ctrl Pts',(-0.384111613704642,32.974926563486,47.9144149636289));
#17646=CARTESIAN_POINT('Ctrl Pts',(-0.544428271512558,32.9777877959916,
47.9224575922029));
#17647=CARTESIAN_POINT('Ctrl Pts',(-0.66105958463499,32.9851160668402,47.9369611544333));
#17648=CARTESIAN_POINT('Ctrl Pts',(-0.959813185315758,33.0169388209901,
47.9956482259754));
#17649=CARTESIAN_POINT('Ctrl Pts',(-1.13654290761119,33.0487223152527,48.0517468025327));
#17650=CARTESIAN_POINT('Ctrl Pts',(-1.61889911237043,33.1675753501152,48.2580271501411));
#17651=CARTESIAN_POINT('Ctrl Pts',(-1.90056409522944,33.2774762837005,48.4455751910135));
#17652=CARTESIAN_POINT('Ctrl Pts',(-2.14849279754675,33.4030003256338,48.658920044375));
#17653=CARTESIAN_POINT('Ctrl Pts',(-46.,55.6250000136559,0.));
#17654=CARTESIAN_POINT('Ctrl Pts',(-46.,55.4166666803226,-12.3256628518316));
#17655=CARTESIAN_POINT('Ctrl Pts',(-39.8371685740842,55.2083333469893,-23.));
#17656=CARTESIAN_POINT('Ctrl Pts',(-33.6743371481684,55.0000000136559,-33.6743371481684));
#17657=CARTESIAN_POINT('Ctrl Pts',(-23.,54.7916666803226,-39.8371685740842));
#17658=CARTESIAN_POINT('Ctrl Pts',(-12.3256628518317,54.5833333469893,-46.));
#17659=CARTESIAN_POINT('Ctrl Pts',(-2.81668763803891E-15,54.3750000136559,
-46.));
#17660=CARTESIAN_POINT('Ctrl Pts',(12.3256628518316,54.1666666803226,-46.));
#17661=CARTESIAN_POINT('Ctrl Pts',(23.,53.9583333469893,-39.8371685740842));
#17662=CARTESIAN_POINT('Ctrl Pts',(33.6743371481683,53.7500000136559,-33.6743371481684));
#17663=CARTESIAN_POINT('Ctrl Pts',(39.8371685740842,53.5416666803226,-23.));
#17664=CARTESIAN_POINT('Ctrl Pts',(46.,53.3333333469893,-12.3256628518317));
#17665=CARTESIAN_POINT('Ctrl Pts',(46.,53.1250000136559,-5.63337527607782E-15));
#17666=CARTESIAN_POINT('Ctrl Pts',(46.,52.9166666803226,12.3256628518316));
#17667=CARTESIAN_POINT('Ctrl Pts',(39.8371685740842,52.7083333469893,23.));
#17668=CARTESIAN_POINT('Ctrl Pts',(33.6743371481684,52.5000000136559,33.6743371481683));
#17669=CARTESIAN_POINT('Ctrl Pts',(23.,52.2916666803226,39.8371685740842));
#17670=CARTESIAN_POINT('Ctrl Pts',(12.3256628518317,52.0833333469893,46.));
#17671=CARTESIAN_POINT('Ctrl Pts',(8.45006291411674E-15,51.8750000136559,
46.));
#17672=CARTESIAN_POINT('Ctrl Pts',(-12.3256628518316,51.6666666803226,46.));
#17673=CARTESIAN_POINT('Ctrl Pts',(-23.,51.4583333469893,39.8371685740842));
#17674=CARTESIAN_POINT('Ctrl Pts',(-33.6743371481683,51.2500000136559,33.6743371481684));
#17675=CARTESIAN_POINT('Ctrl Pts',(-39.8371685740842,51.0416666803226,23.));
#17676=CARTESIAN_POINT('Ctrl Pts',(-46.,50.8333333469893,12.3256628518317));
#17677=CARTESIAN_POINT('Ctrl Pts',(-46.,50.6250000136559,0.));
#17678=CARTESIAN_POINT('Ctrl Pts',(-46.,50.4166666803226,-12.3256628518316));
#17679=CARTESIAN_POINT('Ctrl Pts',(-39.8371685740842,50.2083333469893,-23.));
#17680=CARTESIAN_POINT('Ctrl Pts',(-33.6743371481684,50.0000000136559,-33.6743371481684));
#17681=CARTESIAN_POINT('Ctrl Pts',(-23.,49.7916666803226,-39.8371685740842));
#17682=CARTESIAN_POINT('Ctrl Pts',(-12.3256628518317,49.5833333469893,-46.));
#17683=CARTESIAN_POINT('Ctrl Pts',(-2.81668763803891E-15,49.3750000136559,
-46.));
#17684=CARTESIAN_POINT('Ctrl Pts',(12.3256628518316,49.1666666803226,-46.));
#17685=CARTESIAN_POINT('Ctrl Pts',(23.,48.9583333469893,-39.8371685740842));
#17686=CARTESIAN_POINT('Ctrl Pts',(33.6743371481683,48.7500000136559,-33.6743371481684));
#17687=CARTESIAN_POINT('Ctrl Pts',(39.8371685740842,48.5416666803226,-23.));
#17688=CARTESIAN_POINT('Ctrl Pts',(46.,48.3333333469893,-12.3256628518317));
#17689=CARTESIAN_POINT('Ctrl Pts',(46.,48.1250000136559,-5.63337527607782E-15));
#17690=CARTESIAN_POINT('Ctrl Pts',(46.,47.9166666803226,12.3256628518316));
#17691=CARTESIAN_POINT('Ctrl Pts',(39.8371685740842,47.7083333469893,23.));
#17692=CARTESIAN_POINT('Ctrl Pts',(33.6743371481684,47.5000000136559,33.6743371481683));
#17693=CARTESIAN_POINT('Ctrl Pts',(23.,47.2916666803226,39.8371685740842));
#17694=CARTESIAN_POINT('Ctrl Pts',(12.3256628518317,47.0833333469893,46.));
#17695=CARTESIAN_POINT('Ctrl Pts',(8.45006291411674E-15,46.8750000136559,
46.));
#17696=CARTESIAN_POINT('Ctrl Pts',(-12.3256628518316,46.6666666803226,46.));
#17697=CARTESIAN_POINT('Ctrl Pts',(-23.,46.4583333469893,39.8371685740842));
#17698=CARTESIAN_POINT('Ctrl Pts',(-33.6743371481683,46.2500000136559,33.6743371481684));
#17699=CARTESIAN_POINT('Ctrl Pts',(-39.8371685740842,46.0416666803226,23.));
#17700=CARTESIAN_POINT('Ctrl Pts',(-46.,45.8333333469892,12.3256628518317));
#17701=CARTESIAN_POINT('Ctrl Pts',(-46.,45.6250000136559,0.));
#17702=CARTESIAN_POINT('Ctrl Pts',(-46.,45.4166666803226,-12.3256628518316));
#17703=CARTESIAN_POINT('Ctrl Pts',(-39.8371685740842,45.2083333469893,-23.));
#17704=CARTESIAN_POINT('Ctrl Pts',(-33.6743371481684,45.0000000136559,-33.6743371481684));
#17705=CARTESIAN_POINT('Ctrl Pts',(-23.,44.7916666803226,-39.8371685740842));
#17706=CARTESIAN_POINT('Ctrl Pts',(-12.3256628518317,44.5833333469893,-46.));
#17707=CARTESIAN_POINT('Ctrl Pts',(-2.81668763803891E-15,44.3750000136559,
-46.));
#17708=CARTESIAN_POINT('Ctrl Pts',(12.3256628518316,44.1666666803226,-46.));
#17709=CARTESIAN_POINT('Ctrl Pts',(23.,43.9583333469893,-39.8371685740842));
#17710=CARTESIAN_POINT('Ctrl Pts',(33.6743371481683,43.7500000136559,-33.6743371481684));
#17711=CARTESIAN_POINT('Ctrl Pts',(39.8371685740842,43.5416666803226,-23.));
#17712=CARTESIAN_POINT('Ctrl Pts',(46.,43.3333333469893,-12.3256628518317));
#17713=CARTESIAN_POINT('Ctrl Pts',(46.,43.1250000136559,-5.63337527607782E-15));
#17714=CARTESIAN_POINT('Ctrl Pts',(46.,42.9166666803226,12.3256628518316));
#17715=CARTESIAN_POINT('Ctrl Pts',(39.8371685740842,42.7083333469893,23.));
#17716=CARTESIAN_POINT('Ctrl Pts',(33.6743371481684,42.5000000136559,33.6743371481683));
#17717=CARTESIAN_POINT('Ctrl Pts',(23.,42.2916666803226,39.8371685740842));
#17718=CARTESIAN_POINT('Ctrl Pts',(12.3256628518317,42.0833333469893,46.));
#17719=CARTESIAN_POINT('Ctrl Pts',(8.45006291411674E-15,41.8750000136559,
46.));
#17720=CARTESIAN_POINT('Ctrl Pts',(-12.3256628518316,41.6666666803226,46.));
#17721=CARTESIAN_POINT('Ctrl Pts',(-23.,41.4583333469893,39.8371685740842));
#17722=CARTESIAN_POINT('Ctrl Pts',(-33.6743371481683,41.2500000136559,33.6743371481684));
#17723=CARTESIAN_POINT('Ctrl Pts',(-39.8371685740842,41.0416666803226,23.));
#17724=CARTESIAN_POINT('Ctrl Pts',(-46.,40.8333333469893,12.3256628518317));
#17725=CARTESIAN_POINT('Ctrl Pts',(-46.,40.6250000136559,0.));
#17726=CARTESIAN_POINT('Ctrl Pts',(-46.,40.4166666803226,-12.3256628518316));
#17727=CARTESIAN_POINT('Ctrl Pts',(-39.8371685740842,40.2083333469893,-23.));
#17728=CARTESIAN_POINT('Ctrl Pts',(-33.6743371481684,40.0000000136559,-33.6743371481684));
#17729=CARTESIAN_POINT('Ctrl Pts',(-23.,39.7916666803226,-39.8371685740842));
#17730=CARTESIAN_POINT('Ctrl Pts',(-12.3256628518317,39.5833333469893,-46.));
#17731=CARTESIAN_POINT('Ctrl Pts',(-2.81668763803891E-15,39.3750000136559,
-46.));
#17732=CARTESIAN_POINT('Ctrl Pts',(12.3256628518316,39.1666666803226,-46.));
#17733=CARTESIAN_POINT('Ctrl Pts',(23.,38.9583333469893,-39.8371685740842));
#17734=CARTESIAN_POINT('Ctrl Pts',(33.6743371481683,38.7500000136559,-33.6743371481684));
#17735=CARTESIAN_POINT('Ctrl Pts',(39.8371685740842,38.5416666803226,-23.));
#17736=CARTESIAN_POINT('Ctrl Pts',(46.,38.3333333469893,-12.3256628518317));
#17737=CARTESIAN_POINT('Ctrl Pts',(46.,38.1250000136559,-5.63337527607782E-15));
#17738=CARTESIAN_POINT('Ctrl Pts',(46.,37.9166666803226,12.3256628518316));
#17739=CARTESIAN_POINT('Ctrl Pts',(39.8371685740842,37.7083333469893,23.));
#17740=CARTESIAN_POINT('Ctrl Pts',(33.6743371481684,37.5000000136559,33.6743371481683));
#17741=CARTESIAN_POINT('Ctrl Pts',(23.,37.2916666803226,39.8371685740842));
#17742=CARTESIAN_POINT('Ctrl Pts',(12.3256628518317,37.0833333469893,46.));
#17743=CARTESIAN_POINT('Ctrl Pts',(8.45006291411674E-15,36.8750000136559,
46.));
#17744=CARTESIAN_POINT('Ctrl Pts',(-12.3256628518316,36.6666666803226,46.));
#17745=CARTESIAN_POINT('Ctrl Pts',(-23.,36.4583333469893,39.8371685740842));
#17746=CARTESIAN_POINT('Ctrl Pts',(-33.6743371481683,36.2500000136559,33.6743371481684));
#17747=CARTESIAN_POINT('Ctrl Pts',(-39.8371685740842,36.0416666803226,23.));
#17748=CARTESIAN_POINT('Ctrl Pts',(-46.,35.8333333469893,12.3256628518317));
#17749=CARTESIAN_POINT('Ctrl Pts',(-46.,35.6250000136559,0.));
#17750=CARTESIAN_POINT('Ctrl Pts',(-46.,35.4166666803226,-12.3256628518316));
#17751=CARTESIAN_POINT('Ctrl Pts',(-39.8371685740842,35.2083333469893,-23.));
#17752=CARTESIAN_POINT('Ctrl Pts',(-33.6743371481684,35.0000000136559,-33.6743371481684));
#17753=CARTESIAN_POINT('Ctrl Pts',(-23.,34.7916666803226,-39.8371685740842));
#17754=CARTESIAN_POINT('Ctrl Pts',(-12.3256628518317,34.5833333469893,-46.));
#17755=CARTESIAN_POINT('Ctrl Pts',(-2.81668763803891E-15,34.3750000136559,
-46.));
#17756=CARTESIAN_POINT('Ctrl Pts',(12.3256628518316,34.1666666803226,-46.));
#17757=CARTESIAN_POINT('Ctrl Pts',(23.,33.9583333469893,-39.8371685740842));
#17758=CARTESIAN_POINT('Ctrl Pts',(33.6743371481683,33.7500000136559,-33.6743371481684));
#17759=CARTESIAN_POINT('Ctrl Pts',(39.8371685740842,33.5416666803226,-23.));
#17760=CARTESIAN_POINT('Ctrl Pts',(46.,33.3333333469893,-12.3256628518317));
#17761=CARTESIAN_POINT('Ctrl Pts',(46.,33.1250000136559,-5.63337527607782E-15));
#17762=CARTESIAN_POINT('Ctrl Pts',(46.,32.9166666803226,12.3256628518316));
#17763=CARTESIAN_POINT('Ctrl Pts',(39.8371685740842,32.7083333469893,23.));
#17764=CARTESIAN_POINT('Ctrl Pts',(33.6743371481684,32.5000000136559,33.6743371481683));
#17765=CARTESIAN_POINT('Ctrl Pts',(23.,32.2916666803226,39.8371685740842));
#17766=CARTESIAN_POINT('Ctrl Pts',(12.3256628518317,32.0833333469893,46.));
#17767=CARTESIAN_POINT('Ctrl Pts',(8.45006291411674E-15,31.8750000136559,
46.));
#17768=CARTESIAN_POINT('Ctrl Pts',(-12.3256628518316,31.6666666803226,46.));
#17769=CARTESIAN_POINT('Ctrl Pts',(-23.,31.4583333469893,39.8371685740842));
#17770=CARTESIAN_POINT('Ctrl Pts',(-33.6743371481683,31.2500000136559,33.6743371481684));
#17771=CARTESIAN_POINT('Ctrl Pts',(-39.8371685740842,31.0416666803226,23.));
#17772=CARTESIAN_POINT('Ctrl Pts',(-46.,30.8333333469893,12.3256628518317));
#17773=CARTESIAN_POINT('Ctrl Pts',(-46.,30.6250000136559,0.));
#17774=CARTESIAN_POINT('Ctrl Pts',(-46.,30.4166666803226,-12.3256628518316));
#17775=CARTESIAN_POINT('Ctrl Pts',(-39.8371685740842,30.2083333469893,-23.));
#17776=CARTESIAN_POINT('Ctrl Pts',(-33.6743371481684,30.0000000136559,-33.6743371481684));
#17777=CARTESIAN_POINT('Ctrl Pts',(-23.,29.7916666803226,-39.8371685740842));
#17778=CARTESIAN_POINT('Ctrl Pts',(-12.3256628518317,29.5833333469893,-46.));
#17779=CARTESIAN_POINT('Ctrl Pts',(-2.81668763803891E-15,29.3750000136559,
-46.));
#17780=CARTESIAN_POINT('Ctrl Pts',(12.3256628518316,29.1666666803226,-46.));
#17781=CARTESIAN_POINT('Ctrl Pts',(23.,28.9583333469893,-39.8371685740842));
#17782=CARTESIAN_POINT('Ctrl Pts',(33.6743371481683,28.7500000136559,-33.6743371481684));
#17783=CARTESIAN_POINT('Ctrl Pts',(39.8371685740842,28.5416666803226,-23.));
#17784=CARTESIAN_POINT('Ctrl Pts',(46.,28.3333333469893,-12.3256628518317));
#17785=CARTESIAN_POINT('Ctrl Pts',(46.,28.1250000136559,-5.63337527607782E-15));
#17786=CARTESIAN_POINT('Ctrl Pts',(46.,27.9166666803226,12.3256628518316));
#17787=CARTESIAN_POINT('Ctrl Pts',(39.8371685740842,27.7083333469893,23.));
#17788=CARTESIAN_POINT('Ctrl Pts',(33.6743371481684,27.5000000136559,33.6743371481683));
#17789=CARTESIAN_POINT('Ctrl Pts',(23.,27.2916666803226,39.8371685740842));
#17790=CARTESIAN_POINT('Ctrl Pts',(12.3256628518317,27.0833333469893,46.));
#17791=CARTESIAN_POINT('Ctrl Pts',(8.45006291411674E-15,26.8750000136559,
46.));
#17792=CARTESIAN_POINT('Ctrl Pts',(-12.3256628518316,26.6666666803226,46.));
#17793=CARTESIAN_POINT('Ctrl Pts',(-23.,26.4583333469893,39.8371685740842));
#17794=CARTESIAN_POINT('Ctrl Pts',(-33.6743371481683,26.2500000136559,33.6743371481684));
#17795=CARTESIAN_POINT('Ctrl Pts',(-39.8371685740842,26.0416666803226,23.));
#17796=CARTESIAN_POINT('Ctrl Pts',(-46.,25.8333333469893,12.3256628518317));
#17797=CARTESIAN_POINT('Ctrl Pts',(-46.,25.6250000136559,0.));
#17798=CARTESIAN_POINT('Ctrl Pts',(-48.706329375,57.187500006828,-1.8898197019151E-14));
#17799=CARTESIAN_POINT('Ctrl Pts',(-48.706329375,56.9791666734946,-13.0508216223155));
#17800=CARTESIAN_POINT('Ctrl Pts',(-42.1809185638422,56.7708333401613,-24.3531646875));
#17801=CARTESIAN_POINT('Ctrl Pts',(-35.6555077526845,56.562500006828,-35.6555077526845));
#17802=CARTESIAN_POINT('Ctrl Pts',(-24.3531646875,56.3541666734946,-42.1809185638423));
#17803=CARTESIAN_POINT('Ctrl Pts',(-13.0508216223155,56.1458333401613,-48.706329375));
#17804=CARTESIAN_POINT('Ctrl Pts',(1.59157945007855E-14,55.937500006828,
-48.706329375));
#17805=CARTESIAN_POINT('Ctrl Pts',(13.0508216223155,55.7291666734946,-48.706329375));
#17806=CARTESIAN_POINT('Ctrl Pts',(24.3531646875,55.5208333401613,-42.1809185638422));
#17807=CARTESIAN_POINT('Ctrl Pts',(35.6555077526845,55.312500006828,-35.6555077526845));
#17808=CARTESIAN_POINT('Ctrl Pts',(42.1809185638422,55.1041666734946,-24.3531646875));
#17809=CARTESIAN_POINT('Ctrl Pts',(48.706329375,54.8958333401613,-13.0508216223155));
#17810=CARTESIAN_POINT('Ctrl Pts',(48.706329375,54.687500006828,1.293339198242E-14));
#17811=CARTESIAN_POINT('Ctrl Pts',(48.706329375,54.4791666734946,13.0508216223155));
#17812=CARTESIAN_POINT('Ctrl Pts',(42.1809185638422,54.2708333401613,24.3531646875));
#17813=CARTESIAN_POINT('Ctrl Pts',(35.6555077526845,54.062500006828,35.6555077526845));
#17814=CARTESIAN_POINT('Ctrl Pts',(24.3531646875,53.8541666734946,42.1809185638422));
#17815=CARTESIAN_POINT('Ctrl Pts',(13.0508216223155,53.6458333401613,48.706329375));
#17816=CARTESIAN_POINT('Ctrl Pts',(-9.95098946405443E-15,53.437500006828,
48.706329375));
#17817=CARTESIAN_POINT('Ctrl Pts',(-13.0508216223155,53.2291666734946,48.706329375));
#17818=CARTESIAN_POINT('Ctrl Pts',(-24.3531646875,53.0208333401613,42.1809185638423));
#17819=CARTESIAN_POINT('Ctrl Pts',(-35.6555077526845,52.812500006828,35.6555077526845));
#17820=CARTESIAN_POINT('Ctrl Pts',(-42.1809185638422,52.6041666734946,24.3531646875));
#17821=CARTESIAN_POINT('Ctrl Pts',(-48.706329375,52.3958333401613,13.0508216223155));
#17822=CARTESIAN_POINT('Ctrl Pts',(-48.706329375,52.187500006828,-1.8898197019151E-14));
#17823=CARTESIAN_POINT('Ctrl Pts',(-48.706329375,51.9791666734946,-13.0508216223155));
#17824=CARTESIAN_POINT('Ctrl Pts',(-42.1809185638422,51.7708333401613,-24.3531646875));
#17825=CARTESIAN_POINT('Ctrl Pts',(-35.6555077526845,51.562500006828,-35.6555077526845));
#17826=CARTESIAN_POINT('Ctrl Pts',(-24.3531646875,51.3541666734946,-42.1809185638423));
#17827=CARTESIAN_POINT('Ctrl Pts',(-13.0508216223155,51.1458333401613,-48.706329375));
#17828=CARTESIAN_POINT('Ctrl Pts',(1.59157945007855E-14,50.937500006828,
-48.706329375));
#17829=CARTESIAN_POINT('Ctrl Pts',(13.0508216223155,50.7291666734946,-48.706329375));
#17830=CARTESIAN_POINT('Ctrl Pts',(24.3531646875,50.5208333401613,-42.1809185638422));
#17831=CARTESIAN_POINT('Ctrl Pts',(35.6555077526845,50.312500006828,-35.6555077526845));
#17832=CARTESIAN_POINT('Ctrl Pts',(42.1809185638422,50.1041666734946,-24.3531646875));
#17833=CARTESIAN_POINT('Ctrl Pts',(48.706329375,49.8958333401613,-13.0508216223155));
#17834=CARTESIAN_POINT('Ctrl Pts',(48.706329375,49.687500006828,1.293339198242E-14));
#17835=CARTESIAN_POINT('Ctrl Pts',(48.706329375,49.4791666734946,13.0508216223155));
#17836=CARTESIAN_POINT('Ctrl Pts',(42.1809185638422,49.2708333401613,24.3531646875));
#17837=CARTESIAN_POINT('Ctrl Pts',(35.6555077526845,49.062500006828,35.6555077526845));
#17838=CARTESIAN_POINT('Ctrl Pts',(24.3531646875,48.8541666734946,42.1809185638422));
#17839=CARTESIAN_POINT('Ctrl Pts',(13.0508216223155,48.6458333401613,48.706329375));
#17840=CARTESIAN_POINT('Ctrl Pts',(-9.95098946405443E-15,48.437500006828,
48.706329375));
#17841=CARTESIAN_POINT('Ctrl Pts',(-13.0508216223155,48.2291666734946,48.706329375));
#17842=CARTESIAN_POINT('Ctrl Pts',(-24.3531646875,48.0208333401613,42.1809185638423));
#17843=CARTESIAN_POINT('Ctrl Pts',(-35.6555077526845,47.812500006828,35.6555077526845));
#17844=CARTESIAN_POINT('Ctrl Pts',(-42.1809185638422,47.6041666734946,24.3531646875));
#17845=CARTESIAN_POINT('Ctrl Pts',(-48.706329375,47.3958333401613,13.0508216223155));
#17846=CARTESIAN_POINT('Ctrl Pts',(-48.706329375,47.187500006828,-1.8898197019151E-14));
#17847=CARTESIAN_POINT('Ctrl Pts',(-48.706329375,46.9791666734946,-13.0508216223155));
#17848=CARTESIAN_POINT('Ctrl Pts',(-42.1809185638422,46.7708333401613,-24.3531646875));
#17849=CARTESIAN_POINT('Ctrl Pts',(-35.6555077526845,46.562500006828,-35.6555077526845));
#17850=CARTESIAN_POINT('Ctrl Pts',(-24.3531646875,46.3541666734946,-42.1809185638423));
#17851=CARTESIAN_POINT('Ctrl Pts',(-13.0508216223155,46.1458333401613,-48.706329375));
#17852=CARTESIAN_POINT('Ctrl Pts',(1.59157945007855E-14,45.937500006828,
-48.706329375));
#17853=CARTESIAN_POINT('Ctrl Pts',(13.0508216223155,45.7291666734946,-48.706329375));
#17854=CARTESIAN_POINT('Ctrl Pts',(24.3531646875,45.5208333401613,-42.1809185638422));
#17855=CARTESIAN_POINT('Ctrl Pts',(35.6555077526845,45.312500006828,-35.6555077526845));
#17856=CARTESIAN_POINT('Ctrl Pts',(42.1809185638422,45.1041666734946,-24.3531646875));
#17857=CARTESIAN_POINT('Ctrl Pts',(48.706329375,44.8958333401613,-13.0508216223155));
#17858=CARTESIAN_POINT('Ctrl Pts',(48.706329375,44.687500006828,1.293339198242E-14));
#17859=CARTESIAN_POINT('Ctrl Pts',(48.706329375,44.4791666734946,13.0508216223155));
#17860=CARTESIAN_POINT('Ctrl Pts',(42.1809185638422,44.2708333401613,24.3531646875));
#17861=CARTESIAN_POINT('Ctrl Pts',(35.6555077526845,44.062500006828,35.6555077526845));
#17862=CARTESIAN_POINT('Ctrl Pts',(24.3531646875,43.8541666734946,42.1809185638422));
#17863=CARTESIAN_POINT('Ctrl Pts',(13.0508216223155,43.6458333401613,48.706329375));
#17864=CARTESIAN_POINT('Ctrl Pts',(-9.95098946405443E-15,43.437500006828,
48.706329375));
#17865=CARTESIAN_POINT('Ctrl Pts',(-13.0508216223155,43.2291666734946,48.706329375));
#17866=CARTESIAN_POINT('Ctrl Pts',(-24.3531646875,43.0208333401613,42.1809185638423));
#17867=CARTESIAN_POINT('Ctrl Pts',(-35.6555077526845,42.812500006828,35.6555077526845));
#17868=CARTESIAN_POINT('Ctrl Pts',(-42.1809185638422,42.6041666734946,24.3531646875));
#17869=CARTESIAN_POINT('Ctrl Pts',(-48.706329375,42.3958333401613,13.0508216223155));
#17870=CARTESIAN_POINT('Ctrl Pts',(-48.706329375,42.187500006828,-1.8898197019151E-14));
#17871=CARTESIAN_POINT('Ctrl Pts',(-48.706329375,41.9791666734946,-13.0508216223155));
#17872=CARTESIAN_POINT('Ctrl Pts',(-42.1809185638422,41.7708333401613,-24.3531646875));
#17873=CARTESIAN_POINT('Ctrl Pts',(-35.6555077526845,41.562500006828,-35.6555077526845));
#17874=CARTESIAN_POINT('Ctrl Pts',(-24.3531646875,41.3541666734946,-42.1809185638423));
#17875=CARTESIAN_POINT('Ctrl Pts',(-13.0508216223155,41.1458333401613,-48.706329375));
#17876=CARTESIAN_POINT('Ctrl Pts',(1.59157945007855E-14,40.937500006828,
-48.706329375));
#17877=CARTESIAN_POINT('Ctrl Pts',(13.0508216223155,40.7291666734946,-48.706329375));
#17878=CARTESIAN_POINT('Ctrl Pts',(24.3531646875,40.5208333401613,-42.1809185638422));
#17879=CARTESIAN_POINT('Ctrl Pts',(35.6555077526845,40.312500006828,-35.6555077526845));
#17880=CARTESIAN_POINT('Ctrl Pts',(42.1809185638422,40.1041666734946,-24.3531646875));
#17881=CARTESIAN_POINT('Ctrl Pts',(48.706329375,39.8958333401613,-13.0508216223155));
#17882=CARTESIAN_POINT('Ctrl Pts',(48.706329375,39.687500006828,1.293339198242E-14));
#17883=CARTESIAN_POINT('Ctrl Pts',(48.706329375,39.4791666734946,13.0508216223155));
#17884=CARTESIAN_POINT('Ctrl Pts',(42.1809185638422,39.2708333401613,24.3531646875));
#17885=CARTESIAN_POINT('Ctrl Pts',(35.6555077526845,39.062500006828,35.6555077526845));
#17886=CARTESIAN_POINT('Ctrl Pts',(24.3531646875,38.8541666734946,42.1809185638422));
#17887=CARTESIAN_POINT('Ctrl Pts',(13.0508216223155,38.6458333401613,48.706329375));
#17888=CARTESIAN_POINT('Ctrl Pts',(-9.95098946405443E-15,38.437500006828,
48.706329375));
#17889=CARTESIAN_POINT('Ctrl Pts',(-13.0508216223155,38.2291666734946,48.706329375));
#17890=CARTESIAN_POINT('Ctrl Pts',(-24.3531646875,38.0208333401613,42.1809185638423));
#17891=CARTESIAN_POINT('Ctrl Pts',(-35.6555077526845,37.812500006828,35.6555077526845));
#17892=CARTESIAN_POINT('Ctrl Pts',(-42.1809185638422,37.6041666734946,24.3531646875));
#17893=CARTESIAN_POINT('Ctrl Pts',(-48.706329375,37.3958333401613,13.0508216223155));
#17894=CARTESIAN_POINT('Ctrl Pts',(-48.706329375,37.187500006828,-1.8898197019151E-14));
#17895=CARTESIAN_POINT('Ctrl Pts',(-48.706329375,36.9791666734946,-13.0508216223155));
#17896=CARTESIAN_POINT('Ctrl Pts',(-42.1809185638422,36.7708333401613,-24.3531646875));
#17897=CARTESIAN_POINT('Ctrl Pts',(-35.6555077526845,36.562500006828,-35.6555077526845));
#17898=CARTESIAN_POINT('Ctrl Pts',(-24.3531646875,36.3541666734946,-42.1809185638423));
#17899=CARTESIAN_POINT('Ctrl Pts',(-13.0508216223155,36.1458333401613,-48.706329375));
#17900=CARTESIAN_POINT('Ctrl Pts',(1.59157945007855E-14,35.937500006828,
-48.706329375));
#17901=CARTESIAN_POINT('Ctrl Pts',(13.0508216223155,35.7291666734946,-48.706329375));
#17902=CARTESIAN_POINT('Ctrl Pts',(24.3531646875,35.5208333401613,-42.1809185638422));
#17903=CARTESIAN_POINT('Ctrl Pts',(35.6555077526845,35.312500006828,-35.6555077526845));
#17904=CARTESIAN_POINT('Ctrl Pts',(42.1809185638422,35.1041666734946,-24.3531646875));
#17905=CARTESIAN_POINT('Ctrl Pts',(48.706329375,34.8958333401613,-13.0508216223155));
#17906=CARTESIAN_POINT('Ctrl Pts',(48.706329375,34.687500006828,1.293339198242E-14));
#17907=CARTESIAN_POINT('Ctrl Pts',(48.706329375,34.4791666734946,13.0508216223155));
#17908=CARTESIAN_POINT('Ctrl Pts',(42.1809185638422,34.2708333401613,24.3531646875));
#17909=CARTESIAN_POINT('Ctrl Pts',(35.6555077526845,34.062500006828,35.6555077526845));
#17910=CARTESIAN_POINT('Ctrl Pts',(24.3531646875,33.8541666734946,42.1809185638422));
#17911=CARTESIAN_POINT('Ctrl Pts',(13.0508216223155,33.6458333401613,48.706329375));
#17912=CARTESIAN_POINT('Ctrl Pts',(-9.95098946405443E-15,33.437500006828,
48.706329375));
#17913=CARTESIAN_POINT('Ctrl Pts',(-13.0508216223155,33.2291666734946,48.706329375));
#17914=CARTESIAN_POINT('Ctrl Pts',(-24.3531646875,33.0208333401613,42.1809185638423));
#17915=CARTESIAN_POINT('Ctrl Pts',(-35.6555077526845,32.812500006828,35.6555077526845));
#17916=CARTESIAN_POINT('Ctrl Pts',(-42.1809185638422,32.6041666734946,24.3531646875));
#17917=CARTESIAN_POINT('Ctrl Pts',(-48.706329375,32.3958333401613,13.0508216223155));
#17918=CARTESIAN_POINT('Ctrl Pts',(-48.706329375,32.187500006828,-1.8898197019151E-14));
#17919=CARTESIAN_POINT('Ctrl Pts',(-48.706329375,31.9791666734946,-13.0508216223155));
#17920=CARTESIAN_POINT('Ctrl Pts',(-42.1809185638422,31.7708333401613,-24.3531646875));
#17921=CARTESIAN_POINT('Ctrl Pts',(-35.6555077526845,31.562500006828,-35.6555077526845));
#17922=CARTESIAN_POINT('Ctrl Pts',(-24.3531646875,31.3541666734946,-42.1809185638423));
#17923=CARTESIAN_POINT('Ctrl Pts',(-13.0508216223155,31.1458333401613,-48.706329375));
#17924=CARTESIAN_POINT('Ctrl Pts',(1.59157945007855E-14,30.937500006828,
-48.706329375));
#17925=CARTESIAN_POINT('Ctrl Pts',(13.0508216223155,30.7291666734946,-48.706329375));
#17926=CARTESIAN_POINT('Ctrl Pts',(24.3531646875,30.5208333401613,-42.1809185638422));
#17927=CARTESIAN_POINT('Ctrl Pts',(35.6555077526845,30.312500006828,-35.6555077526845));
#17928=CARTESIAN_POINT('Ctrl Pts',(42.1809185638422,30.1041666734946,-24.3531646875));
#17929=CARTESIAN_POINT('Ctrl Pts',(48.706329375,29.8958333401613,-13.0508216223155));
#17930=CARTESIAN_POINT('Ctrl Pts',(48.706329375,29.687500006828,1.293339198242E-14));
#17931=CARTESIAN_POINT('Ctrl Pts',(48.706329375,29.4791666734946,13.0508216223155));
#17932=CARTESIAN_POINT('Ctrl Pts',(42.1809185638422,29.2708333401613,24.3531646875));
#17933=CARTESIAN_POINT('Ctrl Pts',(35.6555077526845,29.062500006828,35.6555077526845));
#17934=CARTESIAN_POINT('Ctrl Pts',(24.3531646875,28.8541666734946,42.1809185638422));
#17935=CARTESIAN_POINT('Ctrl Pts',(13.0508216223155,28.6458333401613,48.706329375));
#17936=CARTESIAN_POINT('Ctrl Pts',(-9.95098946405443E-15,28.437500006828,
48.706329375));
#17937=CARTESIAN_POINT('Ctrl Pts',(-13.0508216223155,28.2291666734946,48.706329375));
#17938=CARTESIAN_POINT('Ctrl Pts',(-24.3531646875,28.0208333401613,42.1809185638423));
#17939=CARTESIAN_POINT('Ctrl Pts',(-35.6555077526845,27.812500006828,35.6555077526845));
#17940=CARTESIAN_POINT('Ctrl Pts',(-42.1809185638422,27.6041666734946,24.3531646875));
#17941=CARTESIAN_POINT('Ctrl Pts',(-48.706329375,27.3958333401613,13.0508216223155));
#17942=CARTESIAN_POINT('Ctrl Pts',(-48.706329375,27.187500006828,-1.8898197019151E-14));
#17943=CARTESIAN_POINT('',(-48.5134353784345,32.1175463684955,-4.33048599679665));
#17944=CARTESIAN_POINT('',(48.5134353784344,29.7574536451604,-4.33048599679682));
#17945=CARTESIAN_POINT('Ctrl Pts',(-48.5134353784345,32.1175463684955,-4.33048599679665));
#17946=CARTESIAN_POINT('Ctrl Pts',(-47.5573898704235,31.9424850907232,-15.040843219065));
#17947=CARTESIAN_POINT('Ctrl Pts',(-42.1809185638422,31.7708333401613,-24.3531646875));
#17948=CARTESIAN_POINT('Ctrl Pts',(-35.6555077526845,31.562500006828,-35.6555077526845));
#17949=CARTESIAN_POINT('Ctrl Pts',(-24.3531646875,31.3541666734946,-42.1809185638423));
#17950=CARTESIAN_POINT('Ctrl Pts',(-13.0508216223155,31.1458333401613,-48.706329375));
#17951=CARTESIAN_POINT('Ctrl Pts',(1.59157945007855E-14,30.937500006828,
-48.706329375));
#17952=CARTESIAN_POINT('Ctrl Pts',(13.0508216223155,30.7291666734946,-48.706329375));
#17953=CARTESIAN_POINT('Ctrl Pts',(24.3531646875,30.5208333401613,-42.1809185638422));
#17954=CARTESIAN_POINT('Ctrl Pts',(35.6555077526845,30.312500006828,-35.6555077526845));
#17955=CARTESIAN_POINT('Ctrl Pts',(42.1809185638422,30.1041666734946,-24.3531646875));
#17956=CARTESIAN_POINT('Ctrl Pts',(47.5573898704235,29.9325149229327,-15.0408432190651));
#17957=CARTESIAN_POINT('Ctrl Pts',(48.5134353784344,29.7574536451604,-4.33048599679682));
#17958=CARTESIAN_POINT('',(48.235295107789,29.597913825102,-4.33048599679673));
#17959=CARTESIAN_POINT('',(48.5134353784344,29.7574536451604,-4.33048599679682));
#17960=CARTESIAN_POINT('Ctrl Pts',(48.2352951077952,29.5979138250913,-4.33048599679673));
#17961=CARTESIAN_POINT('Ctrl Pts',(47.829636183139,29.3652387164921,-4.33048599679611));
#17962=CARTESIAN_POINT('Ctrl Pts',(47.4228292493871,29.1305469649764,-4.3100254215245));
#17963=CARTESIAN_POINT('Ctrl Pts',(46.6173892826498,28.6628669666112,-4.22607365724017));
#17964=CARTESIAN_POINT('Ctrl Pts',(46.214789133894,28.4275716411426,-4.16216527479196));
#17965=CARTESIAN_POINT('Ctrl Pts',(45.8192253759654,28.1946814357457,-4.07413622090531));
#17966=CARTESIAN_POINT('Ctrl Pts',(-45.7957082162897,30.5508791552084,-4.33048599679682));
#17967=CARTESIAN_POINT('Ctrl Pts',(-46.027322302781,30.6843839384496,-4.33048599679682));
#17968=CARTESIAN_POINT('Ctrl Pts',(-46.4905476657728,30.9513983799647,-4.33048599679661));
#17969=CARTESIAN_POINT('Ctrl Pts',(-46.9537676533565,31.2184221466352,-4.33048599679666));
#17970=CARTESIAN_POINT('Ctrl Pts',(-47.6280672732222,31.6071316973962,-4.33048599679666));
#17971=CARTESIAN_POINT('Ctrl Pts',(-48.0707534890442,31.8623352807796,-4.33048599679665));
#17972=CARTESIAN_POINT('Ctrl Pts',(-48.5134353784345,32.1175463684955,-4.33048599679665));
#17973=CARTESIAN_POINT('Ctrl Pts',(-46.,55.6250000136559,0.));
#17974=CARTESIAN_POINT('Ctrl Pts',(-46.,55.4166666803226,-12.3256628518316));
#17975=CARTESIAN_POINT('Ctrl Pts',(-39.8371685740842,55.2083333469893,-23.));
#17976=CARTESIAN_POINT('Ctrl Pts',(-33.6743371481684,55.0000000136559,-33.6743371481684));
#17977=CARTESIAN_POINT('Ctrl Pts',(-23.,54.7916666803226,-39.8371685740842));
#17978=CARTESIAN_POINT('Ctrl Pts',(-12.3256628518317,54.5833333469893,-46.));
#17979=CARTESIAN_POINT('Ctrl Pts',(-2.81668763803891E-15,54.3750000136559,
-46.));
#17980=CARTESIAN_POINT('Ctrl Pts',(12.3256628518316,54.1666666803226,-46.));
#17981=CARTESIAN_POINT('Ctrl Pts',(23.,53.9583333469893,-39.8371685740842));
#17982=CARTESIAN_POINT('Ctrl Pts',(33.6743371481683,53.7500000136559,-33.6743371481684));
#17983=CARTESIAN_POINT('Ctrl Pts',(39.8371685740842,53.5416666803226,-23.));
#17984=CARTESIAN_POINT('Ctrl Pts',(46.,53.3333333469893,-12.3256628518317));
#17985=CARTESIAN_POINT('Ctrl Pts',(46.,53.1250000136559,-5.63337527607782E-15));
#17986=CARTESIAN_POINT('Ctrl Pts',(46.,52.9166666803226,12.3256628518316));
#17987=CARTESIAN_POINT('Ctrl Pts',(39.8371685740842,52.7083333469893,23.));
#17988=CARTESIAN_POINT('Ctrl Pts',(33.6743371481684,52.5000000136559,33.6743371481683));
#17989=CARTESIAN_POINT('Ctrl Pts',(23.,52.2916666803226,39.8371685740842));
#17990=CARTESIAN_POINT('Ctrl Pts',(12.3256628518317,52.0833333469893,46.));
#17991=CARTESIAN_POINT('Ctrl Pts',(8.45006291411674E-15,51.8750000136559,
46.));
#17992=CARTESIAN_POINT('Ctrl Pts',(-12.3256628518316,51.6666666803226,46.));
#17993=CARTESIAN_POINT('Ctrl Pts',(-23.,51.4583333469893,39.8371685740842));
#17994=CARTESIAN_POINT('Ctrl Pts',(-33.6743371481683,51.2500000136559,33.6743371481684));
#17995=CARTESIAN_POINT('Ctrl Pts',(-39.8371685740842,51.0416666803226,23.));
#17996=CARTESIAN_POINT('Ctrl Pts',(-46.,50.8333333469893,12.3256628518317));
#17997=CARTESIAN_POINT('Ctrl Pts',(-46.,50.6250000136559,0.));
#17998=CARTESIAN_POINT('Ctrl Pts',(-46.,50.4166666803226,-12.3256628518316));
#17999=CARTESIAN_POINT('Ctrl Pts',(-39.8371685740842,50.2083333469893,-23.));
#18000=CARTESIAN_POINT('Ctrl Pts',(-33.6743371481684,50.0000000136559,-33.6743371481684));
#18001=CARTESIAN_POINT('Ctrl Pts',(-23.,49.7916666803226,-39.8371685740842));
#18002=CARTESIAN_POINT('Ctrl Pts',(-12.3256628518317,49.5833333469893,-46.));
#18003=CARTESIAN_POINT('Ctrl Pts',(-2.81668763803891E-15,49.3750000136559,
-46.));
#18004=CARTESIAN_POINT('Ctrl Pts',(12.3256628518316,49.1666666803226,-46.));
#18005=CARTESIAN_POINT('Ctrl Pts',(23.,48.9583333469893,-39.8371685740842));
#18006=CARTESIAN_POINT('Ctrl Pts',(33.6743371481683,48.7500000136559,-33.6743371481684));
#18007=CARTESIAN_POINT('Ctrl Pts',(39.8371685740842,48.5416666803226,-23.));
#18008=CARTESIAN_POINT('Ctrl Pts',(46.,48.3333333469893,-12.3256628518317));
#18009=CARTESIAN_POINT('Ctrl Pts',(46.,48.1250000136559,-5.63337527607782E-15));
#18010=CARTESIAN_POINT('Ctrl Pts',(46.,47.9166666803226,12.3256628518316));
#18011=CARTESIAN_POINT('Ctrl Pts',(39.8371685740842,47.7083333469893,23.));
#18012=CARTESIAN_POINT('Ctrl Pts',(33.6743371481684,47.5000000136559,33.6743371481683));
#18013=CARTESIAN_POINT('Ctrl Pts',(23.,47.2916666803226,39.8371685740842));
#18014=CARTESIAN_POINT('Ctrl Pts',(12.3256628518317,47.0833333469893,46.));
#18015=CARTESIAN_POINT('Ctrl Pts',(8.45006291411674E-15,46.8750000136559,
46.));
#18016=CARTESIAN_POINT('Ctrl Pts',(-12.3256628518316,46.6666666803226,46.));
#18017=CARTESIAN_POINT('Ctrl Pts',(-23.,46.4583333469893,39.8371685740842));
#18018=CARTESIAN_POINT('Ctrl Pts',(-33.6743371481683,46.2500000136559,33.6743371481684));
#18019=CARTESIAN_POINT('Ctrl Pts',(-39.8371685740842,46.0416666803226,23.));
#18020=CARTESIAN_POINT('Ctrl Pts',(-46.,45.8333333469892,12.3256628518317));
#18021=CARTESIAN_POINT('Ctrl Pts',(-46.,45.6250000136559,0.));
#18022=CARTESIAN_POINT('Ctrl Pts',(-46.,45.4166666803226,-12.3256628518316));
#18023=CARTESIAN_POINT('Ctrl Pts',(-39.8371685740842,45.2083333469893,-23.));
#18024=CARTESIAN_POINT('Ctrl Pts',(-33.6743371481684,45.0000000136559,-33.6743371481684));
#18025=CARTESIAN_POINT('Ctrl Pts',(-23.,44.7916666803226,-39.8371685740842));
#18026=CARTESIAN_POINT('Ctrl Pts',(-12.3256628518317,44.5833333469893,-46.));
#18027=CARTESIAN_POINT('Ctrl Pts',(-2.81668763803891E-15,44.3750000136559,
-46.));
#18028=CARTESIAN_POINT('Ctrl Pts',(12.3256628518316,44.1666666803226,-46.));
#18029=CARTESIAN_POINT('Ctrl Pts',(23.,43.9583333469893,-39.8371685740842));
#18030=CARTESIAN_POINT('Ctrl Pts',(33.6743371481683,43.7500000136559,-33.6743371481684));
#18031=CARTESIAN_POINT('Ctrl Pts',(39.8371685740842,43.5416666803226,-23.));
#18032=CARTESIAN_POINT('Ctrl Pts',(46.,43.3333333469893,-12.3256628518317));
#18033=CARTESIAN_POINT('Ctrl Pts',(46.,43.1250000136559,-5.63337527607782E-15));
#18034=CARTESIAN_POINT('Ctrl Pts',(46.,42.9166666803226,12.3256628518316));
#18035=CARTESIAN_POINT('Ctrl Pts',(39.8371685740842,42.7083333469893,23.));
#18036=CARTESIAN_POINT('Ctrl Pts',(33.6743371481684,42.5000000136559,33.6743371481683));
#18037=CARTESIAN_POINT('Ctrl Pts',(23.,42.2916666803226,39.8371685740842));
#18038=CARTESIAN_POINT('Ctrl Pts',(12.3256628518317,42.0833333469893,46.));
#18039=CARTESIAN_POINT('Ctrl Pts',(8.45006291411674E-15,41.8750000136559,
46.));
#18040=CARTESIAN_POINT('Ctrl Pts',(-12.3256628518316,41.6666666803226,46.));
#18041=CARTESIAN_POINT('Ctrl Pts',(-23.,41.4583333469893,39.8371685740842));
#18042=CARTESIAN_POINT('Ctrl Pts',(-33.6743371481683,41.2500000136559,33.6743371481684));
#18043=CARTESIAN_POINT('Ctrl Pts',(-39.8371685740842,41.0416666803226,23.));
#18044=CARTESIAN_POINT('Ctrl Pts',(-46.,40.8333333469893,12.3256628518317));
#18045=CARTESIAN_POINT('Ctrl Pts',(-46.,40.6250000136559,0.));
#18046=CARTESIAN_POINT('Ctrl Pts',(-46.,40.4166666803226,-12.3256628518316));
#18047=CARTESIAN_POINT('Ctrl Pts',(-39.8371685740842,40.2083333469893,-23.));
#18048=CARTESIAN_POINT('Ctrl Pts',(-33.6743371481684,40.0000000136559,-33.6743371481684));
#18049=CARTESIAN_POINT('Ctrl Pts',(-23.,39.7916666803226,-39.8371685740842));
#18050=CARTESIAN_POINT('Ctrl Pts',(-12.3256628518317,39.5833333469893,-46.));
#18051=CARTESIAN_POINT('Ctrl Pts',(-2.81668763803891E-15,39.3750000136559,
-46.));
#18052=CARTESIAN_POINT('Ctrl Pts',(12.3256628518316,39.1666666803226,-46.));
#18053=CARTESIAN_POINT('Ctrl Pts',(23.,38.9583333469893,-39.8371685740842));
#18054=CARTESIAN_POINT('Ctrl Pts',(33.6743371481683,38.7500000136559,-33.6743371481684));
#18055=CARTESIAN_POINT('Ctrl Pts',(39.8371685740842,38.5416666803226,-23.));
#18056=CARTESIAN_POINT('Ctrl Pts',(46.,38.3333333469893,-12.3256628518317));
#18057=CARTESIAN_POINT('Ctrl Pts',(46.,38.1250000136559,-5.63337527607782E-15));
#18058=CARTESIAN_POINT('Ctrl Pts',(46.,37.9166666803226,12.3256628518316));
#18059=CARTESIAN_POINT('Ctrl Pts',(39.8371685740842,37.7083333469893,23.));
#18060=CARTESIAN_POINT('Ctrl Pts',(33.6743371481684,37.5000000136559,33.6743371481683));
#18061=CARTESIAN_POINT('Ctrl Pts',(23.,37.2916666803226,39.8371685740842));
#18062=CARTESIAN_POINT('Ctrl Pts',(12.3256628518317,37.0833333469893,46.));
#18063=CARTESIAN_POINT('Ctrl Pts',(8.45006291411674E-15,36.8750000136559,
46.));
#18064=CARTESIAN_POINT('Ctrl Pts',(-12.3256628518316,36.6666666803226,46.));
#18065=CARTESIAN_POINT('Ctrl Pts',(-23.,36.4583333469893,39.8371685740842));
#18066=CARTESIAN_POINT('Ctrl Pts',(-33.6743371481683,36.2500000136559,33.6743371481684));
#18067=CARTESIAN_POINT('Ctrl Pts',(-39.8371685740842,36.0416666803226,23.));
#18068=CARTESIAN_POINT('Ctrl Pts',(-46.,35.8333333469893,12.3256628518317));
#18069=CARTESIAN_POINT('Ctrl Pts',(-46.,35.6250000136559,0.));
#18070=CARTESIAN_POINT('Ctrl Pts',(-46.,35.4166666803226,-12.3256628518316));
#18071=CARTESIAN_POINT('Ctrl Pts',(-39.8371685740842,35.2083333469893,-23.));
#18072=CARTESIAN_POINT('Ctrl Pts',(-33.6743371481684,35.0000000136559,-33.6743371481684));
#18073=CARTESIAN_POINT('Ctrl Pts',(-23.,34.7916666803226,-39.8371685740842));
#18074=CARTESIAN_POINT('Ctrl Pts',(-12.3256628518317,34.5833333469893,-46.));
#18075=CARTESIAN_POINT('Ctrl Pts',(-2.81668763803891E-15,34.3750000136559,
-46.));
#18076=CARTESIAN_POINT('Ctrl Pts',(12.3256628518316,34.1666666803226,-46.));
#18077=CARTESIAN_POINT('Ctrl Pts',(23.,33.9583333469893,-39.8371685740842));
#18078=CARTESIAN_POINT('Ctrl Pts',(33.6743371481683,33.7500000136559,-33.6743371481684));
#18079=CARTESIAN_POINT('Ctrl Pts',(39.8371685740842,33.5416666803226,-23.));
#18080=CARTESIAN_POINT('Ctrl Pts',(46.,33.3333333469893,-12.3256628518317));
#18081=CARTESIAN_POINT('Ctrl Pts',(46.,33.1250000136559,-5.63337527607782E-15));
#18082=CARTESIAN_POINT('Ctrl Pts',(46.,32.9166666803226,12.3256628518316));
#18083=CARTESIAN_POINT('Ctrl Pts',(39.8371685740842,32.7083333469893,23.));
#18084=CARTESIAN_POINT('Ctrl Pts',(33.6743371481684,32.5000000136559,33.6743371481683));
#18085=CARTESIAN_POINT('Ctrl Pts',(23.,32.2916666803226,39.8371685740842));
#18086=CARTESIAN_POINT('Ctrl Pts',(12.3256628518317,32.0833333469893,46.));
#18087=CARTESIAN_POINT('Ctrl Pts',(8.45006291411674E-15,31.8750000136559,
46.));
#18088=CARTESIAN_POINT('Ctrl Pts',(-12.3256628518316,31.6666666803226,46.));
#18089=CARTESIAN_POINT('Ctrl Pts',(-23.,31.4583333469893,39.8371685740842));
#18090=CARTESIAN_POINT('Ctrl Pts',(-33.6743371481683,31.2500000136559,33.6743371481684));
#18091=CARTESIAN_POINT('Ctrl Pts',(-39.8371685740842,31.0416666803226,23.));
#18092=CARTESIAN_POINT('Ctrl Pts',(-46.,30.8333333469893,12.3256628518317));
#18093=CARTESIAN_POINT('Ctrl Pts',(-46.,30.6250000136559,0.));
#18094=CARTESIAN_POINT('Ctrl Pts',(-46.,30.4166666803226,-12.3256628518316));
#18095=CARTESIAN_POINT('Ctrl Pts',(-39.8371685740842,30.2083333469893,-23.));
#18096=CARTESIAN_POINT('Ctrl Pts',(-33.6743371481684,30.0000000136559,-33.6743371481684));
#18097=CARTESIAN_POINT('Ctrl Pts',(-23.,29.7916666803226,-39.8371685740842));
#18098=CARTESIAN_POINT('Ctrl Pts',(-12.3256628518317,29.5833333469893,-46.));
#18099=CARTESIAN_POINT('Ctrl Pts',(-2.81668763803891E-15,29.3750000136559,
-46.));
#18100=CARTESIAN_POINT('Ctrl Pts',(12.3256628518316,29.1666666803226,-46.));
#18101=CARTESIAN_POINT('Ctrl Pts',(23.,28.9583333469893,-39.8371685740842));
#18102=CARTESIAN_POINT('Ctrl Pts',(33.6743371481683,28.7500000136559,-33.6743371481684));
#18103=CARTESIAN_POINT('Ctrl Pts',(39.8371685740842,28.5416666803226,-23.));
#18104=CARTESIAN_POINT('Ctrl Pts',(46.,28.3333333469893,-12.3256628518317));
#18105=CARTESIAN_POINT('Ctrl Pts',(46.,28.1250000136559,-5.63337527607782E-15));
#18106=CARTESIAN_POINT('Ctrl Pts',(46.,27.9166666803226,12.3256628518316));
#18107=CARTESIAN_POINT('Ctrl Pts',(39.8371685740842,27.7083333469893,23.));
#18108=CARTESIAN_POINT('Ctrl Pts',(33.6743371481684,27.5000000136559,33.6743371481683));
#18109=CARTESIAN_POINT('Ctrl Pts',(23.,27.2916666803226,39.8371685740842));
#18110=CARTESIAN_POINT('Ctrl Pts',(12.3256628518317,27.0833333469893,46.));
#18111=CARTESIAN_POINT('Ctrl Pts',(8.45006291411674E-15,26.8750000136559,
46.));
#18112=CARTESIAN_POINT('Ctrl Pts',(-12.3256628518316,26.6666666803226,46.));
#18113=CARTESIAN_POINT('Ctrl Pts',(-23.,26.4583333469893,39.8371685740842));
#18114=CARTESIAN_POINT('Ctrl Pts',(-33.6743371481683,26.2500000136559,33.6743371481684));
#18115=CARTESIAN_POINT('Ctrl Pts',(-39.8371685740842,26.0416666803226,23.));
#18116=CARTESIAN_POINT('Ctrl Pts',(-46.,25.8333333469893,12.3256628518317));
#18117=CARTESIAN_POINT('Ctrl Pts',(-46.,25.6250000136559,0.));
#18118=CARTESIAN_POINT('Ctrl Pts',(-48.706329375,57.187500006828,-1.8898197019151E-14));
#18119=CARTESIAN_POINT('Ctrl Pts',(-48.706329375,56.9791666734946,-13.0508216223155));
#18120=CARTESIAN_POINT('Ctrl Pts',(-42.1809185638422,56.7708333401613,-24.3531646875));
#18121=CARTESIAN_POINT('Ctrl Pts',(-35.6555077526845,56.562500006828,-35.6555077526845));
#18122=CARTESIAN_POINT('Ctrl Pts',(-24.3531646875,56.3541666734946,-42.1809185638423));
#18123=CARTESIAN_POINT('Ctrl Pts',(-13.0508216223155,56.1458333401613,-48.706329375));
#18124=CARTESIAN_POINT('Ctrl Pts',(1.59157945007855E-14,55.937500006828,
-48.706329375));
#18125=CARTESIAN_POINT('Ctrl Pts',(13.0508216223155,55.7291666734946,-48.706329375));
#18126=CARTESIAN_POINT('Ctrl Pts',(24.3531646875,55.5208333401613,-42.1809185638422));
#18127=CARTESIAN_POINT('Ctrl Pts',(35.6555077526845,55.312500006828,-35.6555077526845));
#18128=CARTESIAN_POINT('Ctrl Pts',(42.1809185638422,55.1041666734946,-24.3531646875));
#18129=CARTESIAN_POINT('Ctrl Pts',(48.706329375,54.8958333401613,-13.0508216223155));
#18130=CARTESIAN_POINT('Ctrl Pts',(48.706329375,54.687500006828,1.293339198242E-14));
#18131=CARTESIAN_POINT('Ctrl Pts',(48.706329375,54.4791666734946,13.0508216223155));
#18132=CARTESIAN_POINT('Ctrl Pts',(42.1809185638422,54.2708333401613,24.3531646875));
#18133=CARTESIAN_POINT('Ctrl Pts',(35.6555077526845,54.062500006828,35.6555077526845));
#18134=CARTESIAN_POINT('Ctrl Pts',(24.3531646875,53.8541666734946,42.1809185638422));
#18135=CARTESIAN_POINT('Ctrl Pts',(13.0508216223155,53.6458333401613,48.706329375));
#18136=CARTESIAN_POINT('Ctrl Pts',(-9.95098946405443E-15,53.437500006828,
48.706329375));
#18137=CARTESIAN_POINT('Ctrl Pts',(-13.0508216223155,53.2291666734946,48.706329375));
#18138=CARTESIAN_POINT('Ctrl Pts',(-24.3531646875,53.0208333401613,42.1809185638423));
#18139=CARTESIAN_POINT('Ctrl Pts',(-35.6555077526845,52.812500006828,35.6555077526845));
#18140=CARTESIAN_POINT('Ctrl Pts',(-42.1809185638422,52.6041666734946,24.3531646875));
#18141=CARTESIAN_POINT('Ctrl Pts',(-48.706329375,52.3958333401613,13.0508216223155));
#18142=CARTESIAN_POINT('Ctrl Pts',(-48.706329375,52.187500006828,-1.8898197019151E-14));
#18143=CARTESIAN_POINT('Ctrl Pts',(-48.706329375,51.9791666734946,-13.0508216223155));
#18144=CARTESIAN_POINT('Ctrl Pts',(-42.1809185638422,51.7708333401613,-24.3531646875));
#18145=CARTESIAN_POINT('Ctrl Pts',(-35.6555077526845,51.562500006828,-35.6555077526845));
#18146=CARTESIAN_POINT('Ctrl Pts',(-24.3531646875,51.3541666734946,-42.1809185638423));
#18147=CARTESIAN_POINT('Ctrl Pts',(-13.0508216223155,51.1458333401613,-48.706329375));
#18148=CARTESIAN_POINT('Ctrl Pts',(1.59157945007855E-14,50.937500006828,
-48.706329375));
#18149=CARTESIAN_POINT('Ctrl Pts',(13.0508216223155,50.7291666734946,-48.706329375));
#18150=CARTESIAN_POINT('Ctrl Pts',(24.3531646875,50.5208333401613,-42.1809185638422));
#18151=CARTESIAN_POINT('Ctrl Pts',(35.6555077526845,50.312500006828,-35.6555077526845));
#18152=CARTESIAN_POINT('Ctrl Pts',(42.1809185638422,50.1041666734946,-24.3531646875));
#18153=CARTESIAN_POINT('Ctrl Pts',(48.706329375,49.8958333401613,-13.0508216223155));
#18154=CARTESIAN_POINT('Ctrl Pts',(48.706329375,49.687500006828,1.293339198242E-14));
#18155=CARTESIAN_POINT('Ctrl Pts',(48.706329375,49.4791666734946,13.0508216223155));
#18156=CARTESIAN_POINT('Ctrl Pts',(42.1809185638422,49.2708333401613,24.3531646875));
#18157=CARTESIAN_POINT('Ctrl Pts',(35.6555077526845,49.062500006828,35.6555077526845));
#18158=CARTESIAN_POINT('Ctrl Pts',(24.3531646875,48.8541666734946,42.1809185638422));
#18159=CARTESIAN_POINT('Ctrl Pts',(13.0508216223155,48.6458333401613,48.706329375));
#18160=CARTESIAN_POINT('Ctrl Pts',(-9.95098946405443E-15,48.437500006828,
48.706329375));
#18161=CARTESIAN_POINT('Ctrl Pts',(-13.0508216223155,48.2291666734946,48.706329375));
#18162=CARTESIAN_POINT('Ctrl Pts',(-24.3531646875,48.0208333401613,42.1809185638423));
#18163=CARTESIAN_POINT('Ctrl Pts',(-35.6555077526845,47.812500006828,35.6555077526845));
#18164=CARTESIAN_POINT('Ctrl Pts',(-42.1809185638422,47.6041666734946,24.3531646875));
#18165=CARTESIAN_POINT('Ctrl Pts',(-48.706329375,47.3958333401613,13.0508216223155));
#18166=CARTESIAN_POINT('Ctrl Pts',(-48.706329375,47.187500006828,-1.8898197019151E-14));
#18167=CARTESIAN_POINT('Ctrl Pts',(-48.706329375,46.9791666734946,-13.0508216223155));
#18168=CARTESIAN_POINT('Ctrl Pts',(-42.1809185638422,46.7708333401613,-24.3531646875));
#18169=CARTESIAN_POINT('Ctrl Pts',(-35.6555077526845,46.562500006828,-35.6555077526845));
#18170=CARTESIAN_POINT('Ctrl Pts',(-24.3531646875,46.3541666734946,-42.1809185638423));
#18171=CARTESIAN_POINT('Ctrl Pts',(-13.0508216223155,46.1458333401613,-48.706329375));
#18172=CARTESIAN_POINT('Ctrl Pts',(1.59157945007855E-14,45.937500006828,
-48.706329375));
#18173=CARTESIAN_POINT('Ctrl Pts',(13.0508216223155,45.7291666734946,-48.706329375));
#18174=CARTESIAN_POINT('Ctrl Pts',(24.3531646875,45.5208333401613,-42.1809185638422));
#18175=CARTESIAN_POINT('Ctrl Pts',(35.6555077526845,45.312500006828,-35.6555077526845));
#18176=CARTESIAN_POINT('Ctrl Pts',(42.1809185638422,45.1041666734946,-24.3531646875));
#18177=CARTESIAN_POINT('Ctrl Pts',(48.706329375,44.8958333401613,-13.0508216223155));
#18178=CARTESIAN_POINT('Ctrl Pts',(48.706329375,44.687500006828,1.293339198242E-14));
#18179=CARTESIAN_POINT('Ctrl Pts',(48.706329375,44.4791666734946,13.0508216223155));
#18180=CARTESIAN_POINT('Ctrl Pts',(42.1809185638422,44.2708333401613,24.3531646875));
#18181=CARTESIAN_POINT('Ctrl Pts',(35.6555077526845,44.062500006828,35.6555077526845));
#18182=CARTESIAN_POINT('Ctrl Pts',(24.3531646875,43.8541666734946,42.1809185638422));
#18183=CARTESIAN_POINT('Ctrl Pts',(13.0508216223155,43.6458333401613,48.706329375));
#18184=CARTESIAN_POINT('Ctrl Pts',(-9.95098946405443E-15,43.437500006828,
48.706329375));
#18185=CARTESIAN_POINT('Ctrl Pts',(-13.0508216223155,43.2291666734946,48.706329375));
#18186=CARTESIAN_POINT('Ctrl Pts',(-24.3531646875,43.0208333401613,42.1809185638423));
#18187=CARTESIAN_POINT('Ctrl Pts',(-35.6555077526845,42.812500006828,35.6555077526845));
#18188=CARTESIAN_POINT('Ctrl Pts',(-42.1809185638422,42.6041666734946,24.3531646875));
#18189=CARTESIAN_POINT('Ctrl Pts',(-48.706329375,42.3958333401613,13.0508216223155));
#18190=CARTESIAN_POINT('Ctrl Pts',(-48.706329375,42.187500006828,-1.8898197019151E-14));
#18191=CARTESIAN_POINT('Ctrl Pts',(-48.706329375,41.9791666734946,-13.0508216223155));
#18192=CARTESIAN_POINT('Ctrl Pts',(-42.1809185638422,41.7708333401613,-24.3531646875));
#18193=CARTESIAN_POINT('Ctrl Pts',(-35.6555077526845,41.562500006828,-35.6555077526845));
#18194=CARTESIAN_POINT('Ctrl Pts',(-24.3531646875,41.3541666734946,-42.1809185638423));
#18195=CARTESIAN_POINT('Ctrl Pts',(-13.0508216223155,41.1458333401613,-48.706329375));
#18196=CARTESIAN_POINT('Ctrl Pts',(1.59157945007855E-14,40.937500006828,
-48.706329375));
#18197=CARTESIAN_POINT('Ctrl Pts',(13.0508216223155,40.7291666734946,-48.706329375));
#18198=CARTESIAN_POINT('Ctrl Pts',(24.3531646875,40.5208333401613,-42.1809185638422));
#18199=CARTESIAN_POINT('Ctrl Pts',(35.6555077526845,40.312500006828,-35.6555077526845));
#18200=CARTESIAN_POINT('Ctrl Pts',(42.1809185638422,40.1041666734946,-24.3531646875));
#18201=CARTESIAN_POINT('Ctrl Pts',(48.706329375,39.8958333401613,-13.0508216223155));
#18202=CARTESIAN_POINT('Ctrl Pts',(48.706329375,39.687500006828,1.293339198242E-14));
#18203=CARTESIAN_POINT('Ctrl Pts',(48.706329375,39.4791666734946,13.0508216223155));
#18204=CARTESIAN_POINT('Ctrl Pts',(42.1809185638422,39.2708333401613,24.3531646875));
#18205=CARTESIAN_POINT('Ctrl Pts',(35.6555077526845,39.062500006828,35.6555077526845));
#18206=CARTESIAN_POINT('Ctrl Pts',(24.3531646875,38.8541666734946,42.1809185638422));
#18207=CARTESIAN_POINT('Ctrl Pts',(13.0508216223155,38.6458333401613,48.706329375));
#18208=CARTESIAN_POINT('Ctrl Pts',(-9.95098946405443E-15,38.437500006828,
48.706329375));
#18209=CARTESIAN_POINT('Ctrl Pts',(-13.0508216223155,38.2291666734946,48.706329375));
#18210=CARTESIAN_POINT('Ctrl Pts',(-24.3531646875,38.0208333401613,42.1809185638423));
#18211=CARTESIAN_POINT('Ctrl Pts',(-35.6555077526845,37.812500006828,35.6555077526845));
#18212=CARTESIAN_POINT('Ctrl Pts',(-42.1809185638422,37.6041666734946,24.3531646875));
#18213=CARTESIAN_POINT('Ctrl Pts',(-48.706329375,37.3958333401613,13.0508216223155));
#18214=CARTESIAN_POINT('Ctrl Pts',(-48.706329375,37.187500006828,-1.8898197019151E-14));
#18215=CARTESIAN_POINT('Ctrl Pts',(-48.706329375,36.9791666734946,-13.0508216223155));
#18216=CARTESIAN_POINT('Ctrl Pts',(-42.1809185638422,36.7708333401613,-24.3531646875));
#18217=CARTESIAN_POINT('Ctrl Pts',(-35.6555077526845,36.562500006828,-35.6555077526845));
#18218=CARTESIAN_POINT('Ctrl Pts',(-24.3531646875,36.3541666734946,-42.1809185638423));
#18219=CARTESIAN_POINT('Ctrl Pts',(-13.0508216223155,36.1458333401613,-48.706329375));
#18220=CARTESIAN_POINT('Ctrl Pts',(1.59157945007855E-14,35.937500006828,
-48.706329375));
#18221=CARTESIAN_POINT('Ctrl Pts',(13.0508216223155,35.7291666734946,-48.706329375));
#18222=CARTESIAN_POINT('Ctrl Pts',(24.3531646875,35.5208333401613,-42.1809185638422));
#18223=CARTESIAN_POINT('Ctrl Pts',(35.6555077526845,35.312500006828,-35.6555077526845));
#18224=CARTESIAN_POINT('Ctrl Pts',(42.1809185638422,35.1041666734946,-24.3531646875));
#18225=CARTESIAN_POINT('Ctrl Pts',(48.706329375,34.8958333401613,-13.0508216223155));
#18226=CARTESIAN_POINT('Ctrl Pts',(48.706329375,34.687500006828,1.293339198242E-14));
#18227=CARTESIAN_POINT('Ctrl Pts',(48.706329375,34.4791666734946,13.0508216223155));
#18228=CARTESIAN_POINT('Ctrl Pts',(42.1809185638422,34.2708333401613,24.3531646875));
#18229=CARTESIAN_POINT('Ctrl Pts',(35.6555077526845,34.062500006828,35.6555077526845));
#18230=CARTESIAN_POINT('Ctrl Pts',(24.3531646875,33.8541666734946,42.1809185638422));
#18231=CARTESIAN_POINT('Ctrl Pts',(13.0508216223155,33.6458333401613,48.706329375));
#18232=CARTESIAN_POINT('Ctrl Pts',(-9.95098946405443E-15,33.437500006828,
48.706329375));
#18233=CARTESIAN_POINT('Ctrl Pts',(-13.0508216223155,33.2291666734946,48.706329375));
#18234=CARTESIAN_POINT('Ctrl Pts',(-24.3531646875,33.0208333401613,42.1809185638423));
#18235=CARTESIAN_POINT('Ctrl Pts',(-35.6555077526845,32.812500006828,35.6555077526845));
#18236=CARTESIAN_POINT('Ctrl Pts',(-42.1809185638422,32.6041666734946,24.3531646875));
#18237=CARTESIAN_POINT('Ctrl Pts',(-48.706329375,32.3958333401613,13.0508216223155));
#18238=CARTESIAN_POINT('Ctrl Pts',(-48.706329375,32.187500006828,-1.8898197019151E-14));
#18239=CARTESIAN_POINT('Ctrl Pts',(-48.706329375,31.9791666734946,-13.0508216223155));
#18240=CARTESIAN_POINT('Ctrl Pts',(-42.1809185638422,31.7708333401613,-24.3531646875));
#18241=CARTESIAN_POINT('Ctrl Pts',(-35.6555077526845,31.562500006828,-35.6555077526845));
#18242=CARTESIAN_POINT('Ctrl Pts',(-24.3531646875,31.3541666734946,-42.1809185638423));
#18243=CARTESIAN_POINT('Ctrl Pts',(-13.0508216223155,31.1458333401613,-48.706329375));
#18244=CARTESIAN_POINT('Ctrl Pts',(1.59157945007855E-14,30.937500006828,
-48.706329375));
#18245=CARTESIAN_POINT('Ctrl Pts',(13.0508216223155,30.7291666734946,-48.706329375));
#18246=CARTESIAN_POINT('Ctrl Pts',(24.3531646875,30.5208333401613,-42.1809185638422));
#18247=CARTESIAN_POINT('Ctrl Pts',(35.6555077526845,30.312500006828,-35.6555077526845));
#18248=CARTESIAN_POINT('Ctrl Pts',(42.1809185638422,30.1041666734946,-24.3531646875));
#18249=CARTESIAN_POINT('Ctrl Pts',(48.706329375,29.8958333401613,-13.0508216223155));
#18250=CARTESIAN_POINT('Ctrl Pts',(48.706329375,29.687500006828,1.293339198242E-14));
#18251=CARTESIAN_POINT('Ctrl Pts',(48.706329375,29.4791666734946,13.0508216223155));
#18252=CARTESIAN_POINT('Ctrl Pts',(42.1809185638422,29.2708333401613,24.3531646875));
#18253=CARTESIAN_POINT('Ctrl Pts',(35.6555077526845,29.062500006828,35.6555077526845));
#18254=CARTESIAN_POINT('Ctrl Pts',(24.3531646875,28.8541666734946,42.1809185638422));
#18255=CARTESIAN_POINT('Ctrl Pts',(13.0508216223155,28.6458333401613,48.706329375));
#18256=CARTESIAN_POINT('Ctrl Pts',(-9.95098946405443E-15,28.437500006828,
48.706329375));
#18257=CARTESIAN_POINT('Ctrl Pts',(-13.0508216223155,28.2291666734946,48.706329375));
#18258=CARTESIAN_POINT('Ctrl Pts',(-24.3531646875,28.0208333401613,42.1809185638423));
#18259=CARTESIAN_POINT('Ctrl Pts',(-35.6555077526845,27.812500006828,35.6555077526845));
#18260=CARTESIAN_POINT('Ctrl Pts',(-42.1809185638422,27.6041666734946,24.3531646875));
#18261=CARTESIAN_POINT('Ctrl Pts',(-48.706329375,27.3958333401613,13.0508216223155));
#18262=CARTESIAN_POINT('Ctrl Pts',(-48.706329375,27.187500006828,-1.8898197019151E-14));
#18263=CARTESIAN_POINT('',(45.8814375100776,28.0686756582683,3.30055934787433));
#18264=CARTESIAN_POINT('',(48.5181022360497,29.5979138251126,3.60701400320334));
#18265=CARTESIAN_POINT('Ctrl Pts',(45.8814375100777,28.0686756582683,3.30055934787429));
#18266=CARTESIAN_POINT('Ctrl Pts',(46.3128558578264,28.3201957499304,3.40558477255907));
#18267=CARTESIAN_POINT('Ctrl Pts',(46.7525547486081,28.5759183229237,3.48196024335446));
#18268=CARTESIAN_POINT('Ctrl Pts',(47.6315848511997,29.085761698813,3.5823978354635));
#18269=CARTESIAN_POINT('Ctrl Pts',(48.0757758296302,29.3427063296139,3.60701400320394));
#18270=CARTESIAN_POINT('Ctrl Pts',(48.5181022360497,29.5979138251126,3.60701400320325));
#18271=CARTESIAN_POINT('',(48.5725845633798,29.6293483229262,3.60701400320327));
#18272=CARTESIAN_POINT('',(48.5181022360497,29.5979138251126,3.60701400320334));
#18273=CARTESIAN_POINT('',(-25.470688436697,28.,41.5156663411139));
#18274=CARTESIAN_POINT('Ctrl Pts',(48.5725845633798,29.6293483229262,3.60701400320327));
#18275=CARTESIAN_POINT('Ctrl Pts',(47.7480251419552,29.4485714020251,14.7106532430575));
#18276=CARTESIAN_POINT('Ctrl Pts',(42.1809185638422,29.2708333401613,24.3531646875));
#18277=CARTESIAN_POINT('Ctrl Pts',(35.6555077526845,29.062500006828,35.6555077526845));
#18278=CARTESIAN_POINT('Ctrl Pts',(24.3531646875,28.8541666734946,42.1809185638422));
#18279=CARTESIAN_POINT('Ctrl Pts',(13.0508216223155,28.6458333401613,48.706329375));
#18280=CARTESIAN_POINT('Ctrl Pts',(-9.95098946405443E-15,28.437500006828,
48.706329375));
#18281=CARTESIAN_POINT('Ctrl Pts',(-13.0508216223155,28.2291666734946,48.706329375));
#18282=CARTESIAN_POINT('Ctrl Pts',(-24.3531646875,28.0208333401613,42.1809185638423));
#18283=CARTESIAN_POINT('Ctrl Pts',(-24.9163678135483,28.0104519542914,41.8557530874098));
#18284=CARTESIAN_POINT('Ctrl Pts',(-25.470688436697,28.,41.5156663411139));
#18285=CARTESIAN_POINT('',(45.4263991839739,28.,7.24170264359533));
#18286=CARTESIAN_POINT('Ctrl Pts',(-25.470688436697,28.,41.5156663411139));
#18287=CARTESIAN_POINT('Ctrl Pts',(-23.6703350842583,28.,42.5523965045972));
#18288=CARTESIAN_POINT('Ctrl Pts',(-21.81189807311,28.0000000000232,43.4701513578078));
#18289=CARTESIAN_POINT('Ctrl Pts',(-18.0206934377531,28.0000000000232,45.0463202583268));
#18290=CARTESIAN_POINT('Ctrl Pts',(-16.1003577817121,28.,45.7062614770701));
#18291=CARTESIAN_POINT('Ctrl Pts',(-10.2442149716332,28.,47.3145402613375));
#18292=CARTESIAN_POINT('Ctrl Pts',(-6.22509096152426,28.,47.8914048604989));
#18293=CARTESIAN_POINT('Ctrl Pts',(-1.01023763277435,28.,47.9805573793013));
#18294=CARTESIAN_POINT('Ctrl Pts',(0.168261352715039,28.,47.9580910618091));
#18295=CARTESIAN_POINT('Ctrl Pts',(7.53171066766197,28.,47.5428134300488));
#18296=CARTESIAN_POINT('Ctrl Pts',(13.5927405733154,28.,45.9875890675615));
#18297=CARTESIAN_POINT('Ctrl Pts',(21.9842976922167,28.,41.975061721578));
#18298=CARTESIAN_POINT('Ctrl Pts',(24.6631550733832,28.,40.3575666553121));
#18299=CARTESIAN_POINT('Ctrl Pts',(31.9704924411577,28.,34.8747898052096));
#18300=CARTESIAN_POINT('Ctrl Pts',(36.0419398812146,28.,30.37145046818));
#18301=CARTESIAN_POINT('Ctrl Pts',(39.9915074797196,28.,23.8278896741577));
#18302=CARTESIAN_POINT('Ctrl Pts',(40.7638953703109,28.,22.3840580410818));
#18303=CARTESIAN_POINT('Ctrl Pts',(43.4788432880031,28.,16.5807834518621));
#18304=CARTESIAN_POINT('Ctrl Pts',(44.8177402925238,28.,11.9727439180169));
#18305=CARTESIAN_POINT('Ctrl Pts',(45.4263991839739,28.,7.24170264359532));
#18306=CARTESIAN_POINT('Origin',(-0.013153225928777,27.9166674358441,-0.0035690946937661));
#18307=CARTESIAN_POINT('Origin',(-7.99360577730113E-14,57.8125000068276,
4.34631818602828E-14));
#18308=CARTESIAN_POINT('',(-3.58014543786854,34.6297857346188,48.5745723586909));
#18309=CARTESIAN_POINT('',(-48.5725845633798,33.4956516907297,3.60701400320325));
#18310=CARTESIAN_POINT('Ctrl Pts',(-3.58014543786854,34.6297857346188,48.5745723586909));
#18311=CARTESIAN_POINT('Ctrl Pts',(-14.6983765927309,34.4487976945266,47.755113069326));
#18312=CARTESIAN_POINT('Ctrl Pts',(-24.3531646875,34.2708333401613,42.1809185638423));
#18313=CARTESIAN_POINT('Ctrl Pts',(-35.6555077526845,34.062500006828,35.6555077526845));
#18314=CARTESIAN_POINT('Ctrl Pts',(-42.1809185638422,33.8541666734946,24.3531646875));
#18315=CARTESIAN_POINT('Ctrl Pts',(-47.7480251419552,33.6764286116308,14.7106532430575));
#18316=CARTESIAN_POINT('Ctrl Pts',(-48.5725845633798,33.4956516907297,3.60701400320325));
#18317=CARTESIAN_POINT('',(-48.5725845633798,33.4956516907297,3.60701400320325));
#18318=CARTESIAN_POINT('Ctrl Pts',(-2.14849279754675,33.4030003256338,48.658920044375));
#18319=CARTESIAN_POINT('Ctrl Pts',(-2.53041200358172,33.5963625381787,48.6420567300503));
#18320=CARTESIAN_POINT('Ctrl Pts',(-2.8769017960051,33.8521925418285,48.6221324989406));
#18321=CARTESIAN_POINT('Ctrl Pts',(-3.31108160489208,34.2864277377636,48.5938831734733));
#18322=CARTESIAN_POINT('Ctrl Pts',(-3.45216898319886,34.4514646385294,48.584004748892));
#18323=CARTESIAN_POINT('Ctrl Pts',(-3.58014543786852,34.6297857346188,48.5745723586909));
#18324=CARTESIAN_POINT('Origin',(-7.99360577730113E-14,57.8125000068276,
4.34631818602828E-14));
#18325=CARTESIAN_POINT('',(-48.5134353784345,33.3675463684955,-4.33048599679665));
#18326=CARTESIAN_POINT('',(48.5134353784344,31.0074536451604,-4.33048599679682));
#18327=CARTESIAN_POINT('Ctrl Pts',(-48.5134353784345,33.3675463684955,-4.33048599679665));
#18328=CARTESIAN_POINT('Ctrl Pts',(-47.5573898704235,33.1924850907233,-15.040843219065));
#18329=CARTESIAN_POINT('Ctrl Pts',(-42.1809185638422,33.0208333401613,-24.3531646875));
#18330=CARTESIAN_POINT('Ctrl Pts',(-35.6555077526845,32.812500006828,-35.6555077526845));
#18331=CARTESIAN_POINT('Ctrl Pts',(-24.3531646875,32.6041666734946,-42.1809185638422));
#18332=CARTESIAN_POINT('Ctrl Pts',(-13.0508216223155,32.3958333401613,-48.706329375));
#18333=CARTESIAN_POINT('Ctrl Pts',(1.59157945007855E-14,32.187500006828,
-48.706329375));
#18334=CARTESIAN_POINT('Ctrl Pts',(13.0508216223155,31.9791666734946,-48.706329375));
#18335=CARTESIAN_POINT('Ctrl Pts',(24.3531646875,31.7708333401613,-42.1809185638422));
#18336=CARTESIAN_POINT('Ctrl Pts',(35.6555077526845,31.562500006828,-35.6555077526845));
#18337=CARTESIAN_POINT('Ctrl Pts',(42.1809185638422,31.3541666734946,-24.3531646875));
#18338=CARTESIAN_POINT('Ctrl Pts',(47.5573898704234,31.1825149229327,-15.0408432190651));
#18339=CARTESIAN_POINT('Ctrl Pts',(48.5134353784344,31.0074536451604,-4.33048599679682));
#18340=CARTESIAN_POINT('',(48.5134353784344,31.0074536451604,-4.33048599679682));
#18341=CARTESIAN_POINT('',(-48.5134353784345,32.1175463684955,-4.33048599679665));
#18342=CARTESIAN_POINT('Origin',(-7.99360577730113E-14,57.8125000068276,
4.34631818602828E-14));
#18343=CARTESIAN_POINT('',(48.5725845633798,30.8793483229262,3.60701400320327));
#18344=CARTESIAN_POINT('',(48.5725845633798,29.6293483229262,3.60701400320327));
#18345=CARTESIAN_POINT('',(-48.5839797682363,28.4930986521586,3.45013493440411));
#18346=CARTESIAN_POINT('Ctrl Pts',(48.5725845633798,30.8793483229262,3.60701400320327));
#18347=CARTESIAN_POINT('Ctrl Pts',(47.7480251419552,30.6985714020251,14.7106532430575));
#18348=CARTESIAN_POINT('Ctrl Pts',(42.1809185638422,30.5208333401613,24.3531646875));
#18349=CARTESIAN_POINT('Ctrl Pts',(35.6555077526845,30.312500006828,35.6555077526845));
#18350=CARTESIAN_POINT('Ctrl Pts',(24.3531646875,30.1041666734946,42.1809185638422));
#18351=CARTESIAN_POINT('Ctrl Pts',(13.0508216223155,29.8958333401613,48.706329375));
#18352=CARTESIAN_POINT('Ctrl Pts',(-9.95098946405443E-15,29.687500006828,
48.706329375));
#18353=CARTESIAN_POINT('Ctrl Pts',(-13.0508216223155,29.4791666734946,48.706329375));
#18354=CARTESIAN_POINT('Ctrl Pts',(-24.3531646875,29.2708333401613,42.1809185638423));
#18355=CARTESIAN_POINT('Ctrl Pts',(-35.6555077526845,29.062500006828,35.6555077526845));
#18356=CARTESIAN_POINT('Ctrl Pts',(-42.1809185638422,28.8541666734946,24.3531646875));
#18357=CARTESIAN_POINT('Ctrl Pts',(-47.7894184949761,28.6751070679821,14.6389578525296));
#18358=CARTESIAN_POINT('Ctrl Pts',(-48.5839797682363,28.4930986521586,3.45013493440411));
#18359=CARTESIAN_POINT('',(-48.5963608758988,28.,3.27112072623103));
#18360=CARTESIAN_POINT('Ctrl Pts',(-48.5839797682365,28.4930986521586,3.45013493440413));
#18361=CARTESIAN_POINT('Ctrl Pts',(-48.5868672036625,28.352811517686,3.40947475531321));
#18362=CARTESIAN_POINT('Ctrl Pts',(-48.5902683144096,28.2142234168628,3.36087918405085));
#18363=CARTESIAN_POINT('Ctrl Pts',(-48.5948275946602,28.0524147745889,3.2938385397297));
#18364=CARTESIAN_POINT('Ctrl Pts',(-48.5955868421039,28.0261433967151,3.28261991219711));
#18365=CARTESIAN_POINT('Ctrl Pts',(-48.5963608758972,28.,3.27112072623101));
#18366=CARTESIAN_POINT('Origin',(7.105427357601E-14,28.0000000000001,-4.66293670342566E-14));
#18367=CARTESIAN_POINT('Ctrl Pts',(-48.706329375,58.437500006828,-1.8898197019151E-14));
#18368=CARTESIAN_POINT('Ctrl Pts',(-48.706329375,58.2291666734946,-13.0508216223155));
#18369=CARTESIAN_POINT('Ctrl Pts',(-42.1809185638422,58.0208333401613,-24.3531646875));
#18370=CARTESIAN_POINT('Ctrl Pts',(-35.6555077526845,57.812500006828,-35.6555077526845));
#18371=CARTESIAN_POINT('Ctrl Pts',(-24.3531646875,57.6041666734946,-42.1809185638422));
#18372=CARTESIAN_POINT('Ctrl Pts',(-13.0508216223155,57.3958333401613,-48.706329375));
#18373=CARTESIAN_POINT('Ctrl Pts',(1.59157945007855E-14,57.187500006828,
-48.706329375));
#18374=CARTESIAN_POINT('Ctrl Pts',(13.0508216223155,56.9791666734946,-48.706329375));
#18375=CARTESIAN_POINT('Ctrl Pts',(24.3531646875,56.7708333401613,-42.1809185638422));
#18376=CARTESIAN_POINT('Ctrl Pts',(35.6555077526845,56.562500006828,-35.6555077526845));
#18377=CARTESIAN_POINT('Ctrl Pts',(42.1809185638422,56.3541666734946,-24.3531646875));
#18378=CARTESIAN_POINT('Ctrl Pts',(48.706329375,56.1458333401613,-13.0508216223155));
#18379=CARTESIAN_POINT('Ctrl Pts',(48.706329375,55.937500006828,1.293339198242E-14));
#18380=CARTESIAN_POINT('Ctrl Pts',(48.706329375,55.7291666734946,13.0508216223155));
#18381=CARTESIAN_POINT('Ctrl Pts',(42.1809185638422,55.5208333401613,24.3531646875));
#18382=CARTESIAN_POINT('Ctrl Pts',(35.6555077526845,55.312500006828,35.6555077526845));
#18383=CARTESIAN_POINT('Ctrl Pts',(24.3531646875,55.1041666734946,42.1809185638422));
#18384=CARTESIAN_POINT('Ctrl Pts',(13.0508216223155,54.8958333401613,48.706329375));
#18385=CARTESIAN_POINT('Ctrl Pts',(-9.95098946405443E-15,54.687500006828,
48.706329375));
#18386=CARTESIAN_POINT('Ctrl Pts',(-13.0508216223155,54.4791666734946,48.706329375));
#18387=CARTESIAN_POINT('Ctrl Pts',(-24.3531646875,54.2708333401613,42.1809185638423));
#18388=CARTESIAN_POINT('Ctrl Pts',(-35.6555077526845,54.062500006828,35.6555077526845));
#18389=CARTESIAN_POINT('Ctrl Pts',(-42.1809185638422,53.8541666734946,24.3531646875));
#18390=CARTESIAN_POINT('Ctrl Pts',(-48.706329375,53.6458333401613,13.0508216223155));
#18391=CARTESIAN_POINT('Ctrl Pts',(-48.706329375,53.437500006828,-1.8898197019151E-14));
#18392=CARTESIAN_POINT('Ctrl Pts',(-48.706329375,53.2291666734946,-13.0508216223155));
#18393=CARTESIAN_POINT('Ctrl Pts',(-42.1809185638422,53.0208333401613,-24.3531646875));
#18394=CARTESIAN_POINT('Ctrl Pts',(-35.6555077526845,52.812500006828,-35.6555077526845));
#18395=CARTESIAN_POINT('Ctrl Pts',(-24.3531646875,52.6041666734946,-42.1809185638422));
#18396=CARTESIAN_POINT('Ctrl Pts',(-13.0508216223155,52.3958333401613,-48.706329375));
#18397=CARTESIAN_POINT('Ctrl Pts',(1.59157945007855E-14,52.187500006828,
-48.706329375));
#18398=CARTESIAN_POINT('Ctrl Pts',(13.0508216223155,51.9791666734946,-48.706329375));
#18399=CARTESIAN_POINT('Ctrl Pts',(24.3531646875,51.7708333401613,-42.1809185638422));
#18400=CARTESIAN_POINT('Ctrl Pts',(35.6555077526845,51.562500006828,-35.6555077526845));
#18401=CARTESIAN_POINT('Ctrl Pts',(42.1809185638422,51.3541666734946,-24.3531646875));
#18402=CARTESIAN_POINT('Ctrl Pts',(48.706329375,51.1458333401613,-13.0508216223155));
#18403=CARTESIAN_POINT('Ctrl Pts',(48.706329375,50.937500006828,1.293339198242E-14));
#18404=CARTESIAN_POINT('Ctrl Pts',(48.706329375,50.7291666734946,13.0508216223155));
#18405=CARTESIAN_POINT('Ctrl Pts',(42.1809185638422,50.5208333401613,24.3531646875));
#18406=CARTESIAN_POINT('Ctrl Pts',(35.6555077526845,50.312500006828,35.6555077526845));
#18407=CARTESIAN_POINT('Ctrl Pts',(24.3531646875,50.1041666734946,42.1809185638422));
#18408=CARTESIAN_POINT('Ctrl Pts',(13.0508216223155,49.8958333401613,48.706329375));
#18409=CARTESIAN_POINT('Ctrl Pts',(-9.95098946405443E-15,49.687500006828,
48.706329375));
#18410=CARTESIAN_POINT('Ctrl Pts',(-13.0508216223155,49.4791666734946,48.706329375));
#18411=CARTESIAN_POINT('Ctrl Pts',(-24.3531646875,49.2708333401613,42.1809185638423));
#18412=CARTESIAN_POINT('Ctrl Pts',(-35.6555077526845,49.062500006828,35.6555077526845));
#18413=CARTESIAN_POINT('Ctrl Pts',(-42.1809185638422,48.8541666734946,24.3531646875));
#18414=CARTESIAN_POINT('Ctrl Pts',(-48.706329375,48.6458333401613,13.0508216223155));
#18415=CARTESIAN_POINT('Ctrl Pts',(-48.706329375,48.437500006828,-1.8898197019151E-14));
#18416=CARTESIAN_POINT('Ctrl Pts',(-48.706329375,48.2291666734946,-13.0508216223155));
#18417=CARTESIAN_POINT('Ctrl Pts',(-42.1809185638422,48.0208333401613,-24.3531646875));
#18418=CARTESIAN_POINT('Ctrl Pts',(-35.6555077526845,47.812500006828,-35.6555077526845));
#18419=CARTESIAN_POINT('Ctrl Pts',(-24.3531646875,47.6041666734946,-42.1809185638422));
#18420=CARTESIAN_POINT('Ctrl Pts',(-13.0508216223155,47.3958333401613,-48.706329375));
#18421=CARTESIAN_POINT('Ctrl Pts',(1.59157945007855E-14,47.187500006828,
-48.706329375));
#18422=CARTESIAN_POINT('Ctrl Pts',(13.0508216223155,46.9791666734946,-48.706329375));
#18423=CARTESIAN_POINT('Ctrl Pts',(24.3531646875,46.7708333401613,-42.1809185638422));
#18424=CARTESIAN_POINT('Ctrl Pts',(35.6555077526845,46.562500006828,-35.6555077526845));
#18425=CARTESIAN_POINT('Ctrl Pts',(42.1809185638422,46.3541666734946,-24.3531646875));
#18426=CARTESIAN_POINT('Ctrl Pts',(48.706329375,46.1458333401613,-13.0508216223155));
#18427=CARTESIAN_POINT('Ctrl Pts',(48.706329375,45.937500006828,1.293339198242E-14));
#18428=CARTESIAN_POINT('Ctrl Pts',(48.706329375,45.7291666734946,13.0508216223155));
#18429=CARTESIAN_POINT('Ctrl Pts',(42.1809185638422,45.5208333401613,24.3531646875));
#18430=CARTESIAN_POINT('Ctrl Pts',(35.6555077526845,45.312500006828,35.6555077526845));
#18431=CARTESIAN_POINT('Ctrl Pts',(24.3531646875,45.1041666734946,42.1809185638422));
#18432=CARTESIAN_POINT('Ctrl Pts',(13.0508216223155,44.8958333401613,48.706329375));
#18433=CARTESIAN_POINT('Ctrl Pts',(-9.95098946405443E-15,44.687500006828,
48.706329375));
#18434=CARTESIAN_POINT('Ctrl Pts',(-13.0508216223155,44.4791666734946,48.706329375));
#18435=CARTESIAN_POINT('Ctrl Pts',(-24.3531646875,44.2708333401613,42.1809185638423));
#18436=CARTESIAN_POINT('Ctrl Pts',(-35.6555077526845,44.062500006828,35.6555077526845));
#18437=CARTESIAN_POINT('Ctrl Pts',(-42.1809185638422,43.8541666734946,24.3531646875));
#18438=CARTESIAN_POINT('Ctrl Pts',(-48.706329375,43.6458333401613,13.0508216223155));
#18439=CARTESIAN_POINT('Ctrl Pts',(-48.706329375,43.437500006828,-1.8898197019151E-14));
#18440=CARTESIAN_POINT('Ctrl Pts',(-48.706329375,43.2291666734946,-13.0508216223155));
#18441=CARTESIAN_POINT('Ctrl Pts',(-42.1809185638422,43.0208333401613,-24.3531646875));
#18442=CARTESIAN_POINT('Ctrl Pts',(-35.6555077526845,42.812500006828,-35.6555077526845));
#18443=CARTESIAN_POINT('Ctrl Pts',(-24.3531646875,42.6041666734946,-42.1809185638422));
#18444=CARTESIAN_POINT('Ctrl Pts',(-13.0508216223155,42.3958333401613,-48.706329375));
#18445=CARTESIAN_POINT('Ctrl Pts',(1.59157945007855E-14,42.187500006828,
-48.706329375));
#18446=CARTESIAN_POINT('Ctrl Pts',(13.0508216223155,41.9791666734946,-48.706329375));
#18447=CARTESIAN_POINT('Ctrl Pts',(24.3531646875,41.7708333401613,-42.1809185638422));
#18448=CARTESIAN_POINT('Ctrl Pts',(35.6555077526845,41.562500006828,-35.6555077526845));
#18449=CARTESIAN_POINT('Ctrl Pts',(42.1809185638422,41.3541666734946,-24.3531646875));
#18450=CARTESIAN_POINT('Ctrl Pts',(48.706329375,41.1458333401613,-13.0508216223155));
#18451=CARTESIAN_POINT('Ctrl Pts',(48.706329375,40.937500006828,1.293339198242E-14));
#18452=CARTESIAN_POINT('Ctrl Pts',(48.706329375,40.7291666734946,13.0508216223155));
#18453=CARTESIAN_POINT('Ctrl Pts',(42.1809185638422,40.5208333401613,24.3531646875));
#18454=CARTESIAN_POINT('Ctrl Pts',(35.6555077526845,40.312500006828,35.6555077526845));
#18455=CARTESIAN_POINT('Ctrl Pts',(24.3531646875,40.1041666734946,42.1809185638422));
#18456=CARTESIAN_POINT('Ctrl Pts',(13.0508216223155,39.8958333401613,48.706329375));
#18457=CARTESIAN_POINT('Ctrl Pts',(-9.95098946405443E-15,39.687500006828,
48.706329375));
#18458=CARTESIAN_POINT('Ctrl Pts',(-13.0508216223155,39.4791666734946,48.706329375));
#18459=CARTESIAN_POINT('Ctrl Pts',(-24.3531646875,39.2708333401613,42.1809185638423));
#18460=CARTESIAN_POINT('Ctrl Pts',(-35.6555077526845,39.062500006828,35.6555077526845));
#18461=CARTESIAN_POINT('Ctrl Pts',(-42.1809185638422,38.8541666734946,24.3531646875));
#18462=CARTESIAN_POINT('Ctrl Pts',(-48.706329375,38.6458333401613,13.0508216223155));
#18463=CARTESIAN_POINT('Ctrl Pts',(-48.706329375,38.437500006828,-1.8898197019151E-14));
#18464=CARTESIAN_POINT('Ctrl Pts',(-48.706329375,38.2291666734946,-13.0508216223155));
#18465=CARTESIAN_POINT('Ctrl Pts',(-42.1809185638422,38.0208333401613,-24.3531646875));
#18466=CARTESIAN_POINT('Ctrl Pts',(-35.6555077526845,37.812500006828,-35.6555077526845));
#18467=CARTESIAN_POINT('Ctrl Pts',(-24.3531646875,37.6041666734946,-42.1809185638422));
#18468=CARTESIAN_POINT('Ctrl Pts',(-13.0508216223155,37.3958333401613,-48.706329375));
#18469=CARTESIAN_POINT('Ctrl Pts',(1.59157945007855E-14,37.187500006828,
-48.706329375));
#18470=CARTESIAN_POINT('Ctrl Pts',(13.0508216223155,36.9791666734946,-48.706329375));
#18471=CARTESIAN_POINT('Ctrl Pts',(24.3531646875,36.7708333401613,-42.1809185638422));
#18472=CARTESIAN_POINT('Ctrl Pts',(35.6555077526845,36.562500006828,-35.6555077526845));
#18473=CARTESIAN_POINT('Ctrl Pts',(42.1809185638422,36.3541666734946,-24.3531646875));
#18474=CARTESIAN_POINT('Ctrl Pts',(48.706329375,36.1458333401613,-13.0508216223155));
#18475=CARTESIAN_POINT('Ctrl Pts',(48.706329375,35.937500006828,1.293339198242E-14));
#18476=CARTESIAN_POINT('Ctrl Pts',(48.706329375,35.7291666734946,13.0508216223155));
#18477=CARTESIAN_POINT('Ctrl Pts',(42.1809185638422,35.5208333401613,24.3531646875));
#18478=CARTESIAN_POINT('Ctrl Pts',(35.6555077526845,35.312500006828,35.6555077526845));
#18479=CARTESIAN_POINT('Ctrl Pts',(24.3531646875,35.1041666734946,42.1809185638422));
#18480=CARTESIAN_POINT('Ctrl Pts',(13.0508216223155,34.8958333401613,48.706329375));
#18481=CARTESIAN_POINT('Ctrl Pts',(-9.95098946405443E-15,34.687500006828,
48.706329375));
#18482=CARTESIAN_POINT('Ctrl Pts',(-13.0508216223155,34.4791666734946,48.706329375));
#18483=CARTESIAN_POINT('Ctrl Pts',(-24.3531646875,34.2708333401613,42.1809185638423));
#18484=CARTESIAN_POINT('Ctrl Pts',(-35.6555077526845,34.062500006828,35.6555077526845));
#18485=CARTESIAN_POINT('Ctrl Pts',(-42.1809185638422,33.8541666734946,24.3531646875));
#18486=CARTESIAN_POINT('Ctrl Pts',(-48.706329375,33.6458333401613,13.0508216223155));
#18487=CARTESIAN_POINT('Ctrl Pts',(-48.706329375,33.437500006828,-1.8898197019151E-14));
#18488=CARTESIAN_POINT('Ctrl Pts',(-48.706329375,33.2291666734946,-13.0508216223155));
#18489=CARTESIAN_POINT('Ctrl Pts',(-42.1809185638422,33.0208333401613,-24.3531646875));
#18490=CARTESIAN_POINT('Ctrl Pts',(-35.6555077526845,32.812500006828,-35.6555077526845));
#18491=CARTESIAN_POINT('Ctrl Pts',(-24.3531646875,32.6041666734946,-42.1809185638422));
#18492=CARTESIAN_POINT('Ctrl Pts',(-13.0508216223155,32.3958333401613,-48.706329375));
#18493=CARTESIAN_POINT('Ctrl Pts',(1.59157945007855E-14,32.187500006828,
-48.706329375));
#18494=CARTESIAN_POINT('Ctrl Pts',(13.0508216223155,31.9791666734946,-48.706329375));
#18495=CARTESIAN_POINT('Ctrl Pts',(24.3531646875,31.7708333401613,-42.1809185638422));
#18496=CARTESIAN_POINT('Ctrl Pts',(35.6555077526845,31.562500006828,-35.6555077526845));
#18497=CARTESIAN_POINT('Ctrl Pts',(42.1809185638422,31.3541666734946,-24.3531646875));
#18498=CARTESIAN_POINT('Ctrl Pts',(48.706329375,31.1458333401613,-13.0508216223155));
#18499=CARTESIAN_POINT('Ctrl Pts',(48.706329375,30.937500006828,1.293339198242E-14));
#18500=CARTESIAN_POINT('Ctrl Pts',(48.706329375,30.7291666734946,13.0508216223155));
#18501=CARTESIAN_POINT('Ctrl Pts',(42.1809185638422,30.5208333401613,24.3531646875));
#18502=CARTESIAN_POINT('Ctrl Pts',(35.6555077526845,30.312500006828,35.6555077526845));
#18503=CARTESIAN_POINT('Ctrl Pts',(24.3531646875,30.1041666734946,42.1809185638422));
#18504=CARTESIAN_POINT('Ctrl Pts',(13.0508216223155,29.8958333401613,48.706329375));
#18505=CARTESIAN_POINT('Ctrl Pts',(-9.95098946405443E-15,29.687500006828,
48.706329375));
#18506=CARTESIAN_POINT('Ctrl Pts',(-13.0508216223155,29.4791666734946,48.706329375));
#18507=CARTESIAN_POINT('Ctrl Pts',(-24.3531646875,29.2708333401613,42.1809185638423));
#18508=CARTESIAN_POINT('Ctrl Pts',(-35.6555077526845,29.062500006828,35.6555077526845));
#18509=CARTESIAN_POINT('Ctrl Pts',(-42.1809185638422,28.8541666734946,24.3531646875));
#18510=CARTESIAN_POINT('Ctrl Pts',(-48.706329375,28.6458333401613,13.0508216223155));
#18511=CARTESIAN_POINT('Ctrl Pts',(-48.706329375,28.437500006828,-1.8898197019151E-14));
#18512=CARTESIAN_POINT('Ctrl Pts',(-45.9999999733281,60.000000015399,1.86248708600067E-22));
#18513=CARTESIAN_POINT('Ctrl Pts',(-45.9999999733281,59.7916666820657,-12.3256628446849));
#18514=CARTESIAN_POINT('Ctrl Pts',(-39.8371685509857,59.5833333487323,-22.9999999866641));
#18515=CARTESIAN_POINT('Ctrl Pts',(-33.6743371286432,59.375000015399,-33.6743371286432));
#18516=CARTESIAN_POINT('Ctrl Pts',(-22.9999999866641,59.1666666820657,-39.8371685509857));
#18517=CARTESIAN_POINT('Ctrl Pts',(-12.3256628446849,58.9583333487323,-45.9999999733281));
#18518=CARTESIAN_POINT('Ctrl Pts',(-2.81668782265444E-15,58.750000015399,
-45.9999999733281));
#18519=CARTESIAN_POINT('Ctrl Pts',(12.3256628446849,58.5416666820657,-45.9999999733281));
#18520=CARTESIAN_POINT('Ctrl Pts',(22.9999999866641,58.3333333487324,-39.8371685509857));
#18521=CARTESIAN_POINT('Ctrl Pts',(33.6743371286432,58.125000015399,-33.6743371286432));
#18522=CARTESIAN_POINT('Ctrl Pts',(39.8371685509856,57.9166666820657,-22.9999999866641));
#18523=CARTESIAN_POINT('Ctrl Pts',(45.9999999733281,57.7083333487323,-12.3256628446849));
#18524=CARTESIAN_POINT('Ctrl Pts',(45.9999999733281,57.500000015399,-5.63337545906017E-15));
#18525=CARTESIAN_POINT('Ctrl Pts',(45.9999999733281,57.2916666820657,12.3256628446849));
#18526=CARTESIAN_POINT('Ctrl Pts',(39.8371685509857,57.0833333487324,22.999999986664));
#18527=CARTESIAN_POINT('Ctrl Pts',(33.6743371286432,56.875000015399,33.6743371286432));
#18528=CARTESIAN_POINT('Ctrl Pts',(22.9999999866641,56.6666666820657,39.8371685509856));
#18529=CARTESIAN_POINT('Ctrl Pts',(12.325662844685,56.4583333487323,45.9999999733281));
#18530=CARTESIAN_POINT('Ctrl Pts',(8.4500630954659E-15,56.250000015399,
45.9999999733281));
#18531=CARTESIAN_POINT('Ctrl Pts',(-12.3256628446849,56.0416666820657,45.9999999733281));
#18532=CARTESIAN_POINT('Ctrl Pts',(-22.999999986664,55.8333333487323,39.8371685509857));
#18533=CARTESIAN_POINT('Ctrl Pts',(-33.6743371286432,55.625000015399,33.6743371286432));
#18534=CARTESIAN_POINT('Ctrl Pts',(-39.8371685509856,55.4166666820657,22.9999999866641));
#18535=CARTESIAN_POINT('Ctrl Pts',(-45.9999999733281,55.2083333487323,12.325662844685));
#18536=CARTESIAN_POINT('Ctrl Pts',(-45.9999999733281,55.000000015399,1.86248708600067E-22));
#18537=CARTESIAN_POINT('Ctrl Pts',(-45.9999999733281,54.7916666820657,-12.3256628446849));
#18538=CARTESIAN_POINT('Ctrl Pts',(-39.8371685509857,54.5833333487323,-22.9999999866641));
#18539=CARTESIAN_POINT('Ctrl Pts',(-33.6743371286432,54.375000015399,-33.6743371286432));
#18540=CARTESIAN_POINT('Ctrl Pts',(-22.9999999866641,54.1666666820657,-39.8371685509857));
#18541=CARTESIAN_POINT('Ctrl Pts',(-12.3256628446849,53.9583333487323,-45.9999999733281));
#18542=CARTESIAN_POINT('Ctrl Pts',(-2.81668782265444E-15,53.750000015399,
-45.9999999733281));
#18543=CARTESIAN_POINT('Ctrl Pts',(12.3256628446849,53.5416666820657,-45.9999999733281));
#18544=CARTESIAN_POINT('Ctrl Pts',(22.9999999866641,53.3333333487323,-39.8371685509857));
#18545=CARTESIAN_POINT('Ctrl Pts',(33.6743371286432,53.125000015399,-33.6743371286432));
#18546=CARTESIAN_POINT('Ctrl Pts',(39.8371685509856,52.9166666820657,-22.9999999866641));
#18547=CARTESIAN_POINT('Ctrl Pts',(45.9999999733281,52.7083333487324,-12.3256628446849));
#18548=CARTESIAN_POINT('Ctrl Pts',(45.9999999733281,52.500000015399,-5.63337545906017E-15));
#18549=CARTESIAN_POINT('Ctrl Pts',(45.9999999733281,52.2916666820657,12.3256628446849));
#18550=CARTESIAN_POINT('Ctrl Pts',(39.8371685509857,52.0833333487323,22.999999986664));
#18551=CARTESIAN_POINT('Ctrl Pts',(33.6743371286432,51.875000015399,33.6743371286432));
#18552=CARTESIAN_POINT('Ctrl Pts',(22.9999999866641,51.6666666820657,39.8371685509856));
#18553=CARTESIAN_POINT('Ctrl Pts',(12.325662844685,51.4583333487323,45.9999999733281));
#18554=CARTESIAN_POINT('Ctrl Pts',(8.4500630954659E-15,51.250000015399,
45.9999999733281));
#18555=CARTESIAN_POINT('Ctrl Pts',(-12.3256628446849,51.0416666820657,45.9999999733281));
#18556=CARTESIAN_POINT('Ctrl Pts',(-22.999999986664,50.8333333487323,39.8371685509857));
#18557=CARTESIAN_POINT('Ctrl Pts',(-33.6743371286432,50.625000015399,33.6743371286432));
#18558=CARTESIAN_POINT('Ctrl Pts',(-39.8371685509856,50.4166666820657,22.9999999866641));
#18559=CARTESIAN_POINT('Ctrl Pts',(-45.9999999733281,50.2083333487323,12.325662844685));
#18560=CARTESIAN_POINT('Ctrl Pts',(-45.9999999733281,50.000000015399,1.86248708600067E-22));
#18561=CARTESIAN_POINT('Ctrl Pts',(-45.9999999733281,49.7916666820657,-12.3256628446849));
#18562=CARTESIAN_POINT('Ctrl Pts',(-39.8371685509857,49.5833333487323,-22.9999999866641));
#18563=CARTESIAN_POINT('Ctrl Pts',(-33.6743371286432,49.375000015399,-33.6743371286432));
#18564=CARTESIAN_POINT('Ctrl Pts',(-22.9999999866641,49.1666666820657,-39.8371685509857));
#18565=CARTESIAN_POINT('Ctrl Pts',(-12.3256628446849,48.9583333487323,-45.9999999733281));
#18566=CARTESIAN_POINT('Ctrl Pts',(-2.81668782265444E-15,48.750000015399,
-45.9999999733281));
#18567=CARTESIAN_POINT('Ctrl Pts',(12.3256628446849,48.5416666820657,-45.9999999733281));
#18568=CARTESIAN_POINT('Ctrl Pts',(22.9999999866641,48.3333333487324,-39.8371685509857));
#18569=CARTESIAN_POINT('Ctrl Pts',(33.6743371286432,48.125000015399,-33.6743371286432));
#18570=CARTESIAN_POINT('Ctrl Pts',(39.8371685509856,47.9166666820657,-22.9999999866641));
#18571=CARTESIAN_POINT('Ctrl Pts',(45.9999999733281,47.7083333487324,-12.3256628446849));
#18572=CARTESIAN_POINT('Ctrl Pts',(45.9999999733281,47.500000015399,-5.63337545906017E-15));
#18573=CARTESIAN_POINT('Ctrl Pts',(45.9999999733281,47.2916666820657,12.3256628446849));
#18574=CARTESIAN_POINT('Ctrl Pts',(39.8371685509857,47.0833333487323,22.999999986664));
#18575=CARTESIAN_POINT('Ctrl Pts',(33.6743371286432,46.875000015399,33.6743371286432));
#18576=CARTESIAN_POINT('Ctrl Pts',(22.9999999866641,46.6666666820657,39.8371685509856));
#18577=CARTESIAN_POINT('Ctrl Pts',(12.325662844685,46.4583333487324,45.9999999733281));
#18578=CARTESIAN_POINT('Ctrl Pts',(8.4500630954659E-15,46.250000015399,
45.9999999733281));
#18579=CARTESIAN_POINT('Ctrl Pts',(-12.3256628446849,46.0416666820657,45.9999999733281));
#18580=CARTESIAN_POINT('Ctrl Pts',(-22.999999986664,45.8333333487323,39.8371685509857));
#18581=CARTESIAN_POINT('Ctrl Pts',(-33.6743371286432,45.625000015399,33.6743371286432));
#18582=CARTESIAN_POINT('Ctrl Pts',(-39.8371685509856,45.4166666820657,22.9999999866641));
#18583=CARTESIAN_POINT('Ctrl Pts',(-45.9999999733281,45.2083333487323,12.325662844685));
#18584=CARTESIAN_POINT('Ctrl Pts',(-45.9999999733281,45.000000015399,1.86248708600067E-22));
#18585=CARTESIAN_POINT('Ctrl Pts',(-45.9999999733281,44.7916666820657,-12.3256628446849));
#18586=CARTESIAN_POINT('Ctrl Pts',(-39.8371685509857,44.5833333487323,-22.9999999866641));
#18587=CARTESIAN_POINT('Ctrl Pts',(-33.6743371286432,44.375000015399,-33.6743371286432));
#18588=CARTESIAN_POINT('Ctrl Pts',(-22.9999999866641,44.1666666820657,-39.8371685509857));
#18589=CARTESIAN_POINT('Ctrl Pts',(-12.3256628446849,43.9583333487323,-45.9999999733281));
#18590=CARTESIAN_POINT('Ctrl Pts',(-2.81668782265444E-15,43.750000015399,
-45.9999999733281));
#18591=CARTESIAN_POINT('Ctrl Pts',(12.3256628446849,43.5416666820657,-45.9999999733281));
#18592=CARTESIAN_POINT('Ctrl Pts',(22.9999999866641,43.3333333487324,-39.8371685509857));
#18593=CARTESIAN_POINT('Ctrl Pts',(33.6743371286432,43.125000015399,-33.6743371286432));
#18594=CARTESIAN_POINT('Ctrl Pts',(39.8371685509856,42.9166666820657,-22.9999999866641));
#18595=CARTESIAN_POINT('Ctrl Pts',(45.9999999733281,42.7083333487324,-12.3256628446849));
#18596=CARTESIAN_POINT('Ctrl Pts',(45.9999999733281,42.500000015399,-5.63337545906017E-15));
#18597=CARTESIAN_POINT('Ctrl Pts',(45.9999999733281,42.2916666820657,12.3256628446849));
#18598=CARTESIAN_POINT('Ctrl Pts',(39.8371685509857,42.0833333487324,22.999999986664));
#18599=CARTESIAN_POINT('Ctrl Pts',(33.6743371286432,41.875000015399,33.6743371286432));
#18600=CARTESIAN_POINT('Ctrl Pts',(22.9999999866641,41.6666666820657,39.8371685509856));
#18601=CARTESIAN_POINT('Ctrl Pts',(12.325662844685,41.4583333487323,45.9999999733281));
#18602=CARTESIAN_POINT('Ctrl Pts',(8.4500630954659E-15,41.250000015399,
45.9999999733281));
#18603=CARTESIAN_POINT('Ctrl Pts',(-12.3256628446849,41.0416666820657,45.9999999733281));
#18604=CARTESIAN_POINT('Ctrl Pts',(-22.999999986664,40.8333333487324,39.8371685509857));
#18605=CARTESIAN_POINT('Ctrl Pts',(-33.6743371286432,40.625000015399,33.6743371286432));
#18606=CARTESIAN_POINT('Ctrl Pts',(-39.8371685509856,40.4166666820657,22.9999999866641));
#18607=CARTESIAN_POINT('Ctrl Pts',(-45.9999999733281,40.2083333487324,12.325662844685));
#18608=CARTESIAN_POINT('Ctrl Pts',(-45.9999999733281,40.000000015399,1.86248708600067E-22));
#18609=CARTESIAN_POINT('Ctrl Pts',(-45.9999999733281,39.7916666820657,-12.3256628446849));
#18610=CARTESIAN_POINT('Ctrl Pts',(-39.8371685509857,39.5833333487323,-22.9999999866641));
#18611=CARTESIAN_POINT('Ctrl Pts',(-33.6743371286432,39.375000015399,-33.6743371286432));
#18612=CARTESIAN_POINT('Ctrl Pts',(-22.9999999866641,39.1666666820657,-39.8371685509857));
#18613=CARTESIAN_POINT('Ctrl Pts',(-12.3256628446849,38.9583333487323,-45.9999999733281));
#18614=CARTESIAN_POINT('Ctrl Pts',(-2.81668782265444E-15,38.750000015399,
-45.9999999733281));
#18615=CARTESIAN_POINT('Ctrl Pts',(12.3256628446849,38.5416666820657,-45.9999999733281));
#18616=CARTESIAN_POINT('Ctrl Pts',(22.9999999866641,38.3333333487323,-39.8371685509857));
#18617=CARTESIAN_POINT('Ctrl Pts',(33.6743371286432,38.125000015399,-33.6743371286432));
#18618=CARTESIAN_POINT('Ctrl Pts',(39.8371685509856,37.9166666820657,-22.9999999866641));
#18619=CARTESIAN_POINT('Ctrl Pts',(45.9999999733281,37.7083333487323,-12.3256628446849));
#18620=CARTESIAN_POINT('Ctrl Pts',(45.9999999733281,37.500000015399,-5.63337545906017E-15));
#18621=CARTESIAN_POINT('Ctrl Pts',(45.9999999733281,37.2916666820657,12.3256628446849));
#18622=CARTESIAN_POINT('Ctrl Pts',(39.8371685509857,37.0833333487323,22.999999986664));
#18623=CARTESIAN_POINT('Ctrl Pts',(33.6743371286432,36.875000015399,33.6743371286432));
#18624=CARTESIAN_POINT('Ctrl Pts',(22.9999999866641,36.6666666820657,39.8371685509856));
#18625=CARTESIAN_POINT('Ctrl Pts',(12.325662844685,36.4583333487323,45.9999999733281));
#18626=CARTESIAN_POINT('Ctrl Pts',(8.4500630954659E-15,36.250000015399,
45.9999999733281));
#18627=CARTESIAN_POINT('Ctrl Pts',(-12.3256628446849,36.0416666820657,45.9999999733281));
#18628=CARTESIAN_POINT('Ctrl Pts',(-22.999999986664,35.8333333487323,39.8371685509857));
#18629=CARTESIAN_POINT('Ctrl Pts',(-33.6743371286432,35.625000015399,33.6743371286432));
#18630=CARTESIAN_POINT('Ctrl Pts',(-39.8371685509856,35.4166666820657,22.9999999866641));
#18631=CARTESIAN_POINT('Ctrl Pts',(-45.9999999733281,35.2083333487323,12.325662844685));
#18632=CARTESIAN_POINT('Ctrl Pts',(-45.9999999733281,35.000000015399,1.86248708600067E-22));
#18633=CARTESIAN_POINT('Ctrl Pts',(-45.9999999733281,34.7916666820657,-12.3256628446849));
#18634=CARTESIAN_POINT('Ctrl Pts',(-39.8371685509857,34.5833333487323,-22.9999999866641));
#18635=CARTESIAN_POINT('Ctrl Pts',(-33.6743371286432,34.375000015399,-33.6743371286432));
#18636=CARTESIAN_POINT('Ctrl Pts',(-22.9999999866641,34.1666666820657,-39.8371685509857));
#18637=CARTESIAN_POINT('Ctrl Pts',(-12.3256628446849,33.9583333487323,-45.9999999733281));
#18638=CARTESIAN_POINT('Ctrl Pts',(-2.81668782265444E-15,33.750000015399,
-45.9999999733281));
#18639=CARTESIAN_POINT('Ctrl Pts',(12.3256628446849,33.5416666820657,-45.9999999733281));
#18640=CARTESIAN_POINT('Ctrl Pts',(22.9999999866641,33.3333333487323,-39.8371685509857));
#18641=CARTESIAN_POINT('Ctrl Pts',(33.6743371286432,33.125000015399,-33.6743371286432));
#18642=CARTESIAN_POINT('Ctrl Pts',(39.8371685509856,32.9166666820657,-22.9999999866641));
#18643=CARTESIAN_POINT('Ctrl Pts',(45.9999999733281,32.7083333487323,-12.3256628446849));
#18644=CARTESIAN_POINT('Ctrl Pts',(45.9999999733281,32.500000015399,-5.63337545906017E-15));
#18645=CARTESIAN_POINT('Ctrl Pts',(45.9999999733281,32.2916666820657,12.3256628446849));
#18646=CARTESIAN_POINT('Ctrl Pts',(39.8371685509857,32.0833333487323,22.999999986664));
#18647=CARTESIAN_POINT('Ctrl Pts',(33.6743371286432,31.875000015399,33.6743371286432));
#18648=CARTESIAN_POINT('Ctrl Pts',(22.9999999866641,31.6666666820657,39.8371685509856));
#18649=CARTESIAN_POINT('Ctrl Pts',(12.325662844685,31.4583333487323,45.9999999733281));
#18650=CARTESIAN_POINT('Ctrl Pts',(8.4500630954659E-15,31.250000015399,
45.9999999733281));
#18651=CARTESIAN_POINT('Ctrl Pts',(-12.3256628446849,31.0416666820657,45.9999999733281));
#18652=CARTESIAN_POINT('Ctrl Pts',(-22.999999986664,30.8333333487323,39.8371685509857));
#18653=CARTESIAN_POINT('Ctrl Pts',(-33.6743371286432,30.625000015399,33.6743371286432));
#18654=CARTESIAN_POINT('Ctrl Pts',(-39.8371685509856,30.4166666820657,22.9999999866641));
#18655=CARTESIAN_POINT('Ctrl Pts',(-45.9999999733281,30.2083333487323,12.325662844685));
#18656=CARTESIAN_POINT('Ctrl Pts',(-45.9999999733281,30.000000015399,1.86248708600067E-22));
#18657=CARTESIAN_POINT('Ctrl Pts',(45.7957082162897,32.5741208584476,-4.33048599679664));
#18658=CARTESIAN_POINT('Ctrl Pts',(46.027322302781,32.4406160752063,-4.33048599679664));
#18659=CARTESIAN_POINT('Ctrl Pts',(46.4905476657728,32.1736016336912,-4.33048599679679));
#18660=CARTESIAN_POINT('Ctrl Pts',(46.9537676533565,31.9065778670208,-4.33048599679665));
#18661=CARTESIAN_POINT('Ctrl Pts',(47.6280672732222,31.5178683162597,-4.33048599679665));
#18662=CARTESIAN_POINT('Ctrl Pts',(48.0707534890442,31.2626647328764,-4.33048599679682));
#18663=CARTESIAN_POINT('Ctrl Pts',(48.5134353784344,31.0074536451604,-4.33048599679682));
#18664=CARTESIAN_POINT('Origin',(4513.80899750787,-7920.15854999024,-4.33048586364984));
#18665=CARTESIAN_POINT('Ctrl Pts',(-2.77456427460704,33.7972761197826,-45.9162475937012));
#18666=CARTESIAN_POINT('Ctrl Pts',(-2.63312591332868,33.6885519019789,-46.1089077818654));
#18667=CARTESIAN_POINT('Ctrl Pts',(-2.47630178223139,33.5831756620264,-46.2955459160921));
#18668=CARTESIAN_POINT('Ctrl Pts',(-2.09992691815342,33.371173761156,-46.6702834188207));
#18669=CARTESIAN_POINT('Ctrl Pts',(-1.86960700461488,33.2651451031817,-46.8571879502895));
#18670=CARTESIAN_POINT('Ctrl Pts',(-1.44126400733626,33.1220740404168,-47.1072221114464));
#18671=CARTESIAN_POINT('Ctrl Pts',(-1.25731789418526,33.0737193247225,-47.1910001179499));
#18672=CARTESIAN_POINT('Ctrl Pts',(-0.930990574714349,33.0146873105689,
-47.291192418918));
#18673=CARTESIAN_POINT('Ctrl Pts',(-0.79608853305349,32.9971216590757,-47.3202305438409));
#18674=CARTESIAN_POINT('Ctrl Pts',(-0.593494556430455,32.9816476890939,
-47.3440578144643));
#18675=CARTESIAN_POINT('Ctrl Pts',(-0.528604008161592,32.9782810542056,
-47.3488063321149));
#18676=CARTESIAN_POINT('Ctrl Pts',(-0.455514956847433,32.9762981123005,
-47.3508718861098));
#18677=CARTESIAN_POINT('Ctrl Pts',(-0.447577390437119,32.9761065917277,
-47.3510529648804));
#18678=CARTESIAN_POINT('Ctrl Pts',(-0.43531402020566,32.9758475255699,-47.3512658915012));
#18679=CARTESIAN_POINT('Ctrl Pts',(-0.430989393289628,32.9757632392308,
-47.3513281446522));
#18680=CARTESIAN_POINT('Ctrl Pts',(-0.425732734692202,32.9756693851213,
-47.3513882117866));
#18681=CARTESIAN_POINT('Ctrl Pts',(-0.424801004760669,32.9756530779659,
-47.3513982628154));
#18682=CARTESIAN_POINT('Ctrl Pts',(-0.423270430619263,32.9756268290707,
-47.3514137952413));
#18683=CARTESIAN_POINT('Ctrl Pts',(-0.42267159374665,32.9756166947886,-47.3514196262221));
#18684=CARTESIAN_POINT('Ctrl Pts',(-0.421601003469021,32.9755988193071,
-47.3514296108102));
#18685=CARTESIAN_POINT('Ctrl Pts',(-0.421129251994336,32.9755910266925,
-47.3514338577676));
#18686=CARTESIAN_POINT('Ctrl Pts',(-0.420123704778293,32.9755745959494,
-47.3514425847247));
#18687=CARTESIAN_POINT('Ctrl Pts',(-0.419589908379852,32.9755659813974,
-47.3514470219234));
#18688=CARTESIAN_POINT('Ctrl Pts',(-0.418167541624201,32.9755433139297,
-47.3514583243956));
#18689=CARTESIAN_POINT('Ctrl Pts',(-0.417278965930535,32.9755294517199,
-47.351464843457));
#18690=CARTESIAN_POINT('Ctrl Pts',(-0.4131415843562,32.9754662965793,-47.3514926748277));
#18691=CARTESIAN_POINT('Ctrl Pts',(-0.409892694872467,32.9754206944094,
-47.3515072872273));
#18692=CARTESIAN_POINT('Ctrl Pts',(-0.386060814153076,32.9751154571127,
-47.3515613489623));
#18693=CARTESIAN_POINT('Ctrl Pts',(-0.365479633441874,32.9750120157055,
-47.3513173638308));
#18694=CARTESIAN_POINT('Ctrl Pts',(-0.26272690047942,32.9752945949283,-47.3486490070669));
#18695=CARTESIAN_POINT('Ctrl Pts',(-0.180951746939931,32.9780716383461,
-47.3418930110935));
#18696=CARTESIAN_POINT('Ctrl Pts',(0.0529660757825567,32.9931992298982,
-47.309526490652));
#18697=CARTESIAN_POINT('Ctrl Pts',(0.201533978643987,33.0116665859949,-47.2728828889392));
#18698=CARTESIAN_POINT('Ctrl Pts',(0.553021373295282,33.0747615694622,-47.1509572093954));
#18699=CARTESIAN_POINT('Ctrl Pts',(0.747612808578448,33.1267664634886,-47.0524625034721));
#18700=CARTESIAN_POINT('Ctrl Pts',(1.29390814642398,33.3135276394169,-46.7021675926803));
#18701=CARTESIAN_POINT('Ctrl Pts',(1.63924643152126,33.4911286721254,-46.3728987766334));
#18702=CARTESIAN_POINT('Ctrl Pts',(1.95443836226863,33.716777165276,-45.958461361191));
#18703=CARTESIAN_POINT('Ctrl Pts',(-48.706329375,58.437500006828,-1.8898197019151E-14));
#18704=CARTESIAN_POINT('Ctrl Pts',(-48.706329375,58.2291666734946,-13.0508216223155));
#18705=CARTESIAN_POINT('Ctrl Pts',(-42.1809185638422,58.0208333401613,-24.3531646875));
#18706=CARTESIAN_POINT('Ctrl Pts',(-35.6555077526845,57.812500006828,-35.6555077526845));
#18707=CARTESIAN_POINT('Ctrl Pts',(-24.3531646875,57.6041666734946,-42.1809185638422));
#18708=CARTESIAN_POINT('Ctrl Pts',(-13.0508216223155,57.3958333401613,-48.706329375));
#18709=CARTESIAN_POINT('Ctrl Pts',(1.59157945007855E-14,57.187500006828,
-48.706329375));
#18710=CARTESIAN_POINT('Ctrl Pts',(13.0508216223155,56.9791666734946,-48.706329375));
#18711=CARTESIAN_POINT('Ctrl Pts',(24.3531646875,56.7708333401613,-42.1809185638422));
#18712=CARTESIAN_POINT('Ctrl Pts',(35.6555077526845,56.562500006828,-35.6555077526845));
#18713=CARTESIAN_POINT('Ctrl Pts',(42.1809185638422,56.3541666734946,-24.3531646875));
#18714=CARTESIAN_POINT('Ctrl Pts',(48.706329375,56.1458333401613,-13.0508216223155));
#18715=CARTESIAN_POINT('Ctrl Pts',(48.706329375,55.937500006828,1.293339198242E-14));
#18716=CARTESIAN_POINT('Ctrl Pts',(48.706329375,55.7291666734946,13.0508216223155));
#18717=CARTESIAN_POINT('Ctrl Pts',(42.1809185638422,55.5208333401613,24.3531646875));
#18718=CARTESIAN_POINT('Ctrl Pts',(35.6555077526845,55.312500006828,35.6555077526845));
#18719=CARTESIAN_POINT('Ctrl Pts',(24.3531646875,55.1041666734946,42.1809185638422));
#18720=CARTESIAN_POINT('Ctrl Pts',(13.0508216223155,54.8958333401613,48.706329375));
#18721=CARTESIAN_POINT('Ctrl Pts',(-9.95098946405443E-15,54.687500006828,
48.706329375));
#18722=CARTESIAN_POINT('Ctrl Pts',(-13.0508216223155,54.4791666734946,48.706329375));
#18723=CARTESIAN_POINT('Ctrl Pts',(-24.3531646875,54.2708333401613,42.1809185638423));
#18724=CARTESIAN_POINT('Ctrl Pts',(-35.6555077526845,54.062500006828,35.6555077526845));
#18725=CARTESIAN_POINT('Ctrl Pts',(-42.1809185638422,53.8541666734946,24.3531646875));
#18726=CARTESIAN_POINT('Ctrl Pts',(-48.706329375,53.6458333401613,13.0508216223155));
#18727=CARTESIAN_POINT('Ctrl Pts',(-48.706329375,53.437500006828,-1.8898197019151E-14));
#18728=CARTESIAN_POINT('Ctrl Pts',(-48.706329375,53.2291666734946,-13.0508216223155));
#18729=CARTESIAN_POINT('Ctrl Pts',(-42.1809185638422,53.0208333401613,-24.3531646875));
#18730=CARTESIAN_POINT('Ctrl Pts',(-35.6555077526845,52.812500006828,-35.6555077526845));
#18731=CARTESIAN_POINT('Ctrl Pts',(-24.3531646875,52.6041666734946,-42.1809185638422));
#18732=CARTESIAN_POINT('Ctrl Pts',(-13.0508216223155,52.3958333401613,-48.706329375));
#18733=CARTESIAN_POINT('Ctrl Pts',(1.59157945007855E-14,52.187500006828,
-48.706329375));
#18734=CARTESIAN_POINT('Ctrl Pts',(13.0508216223155,51.9791666734946,-48.706329375));
#18735=CARTESIAN_POINT('Ctrl Pts',(24.3531646875,51.7708333401613,-42.1809185638422));
#18736=CARTESIAN_POINT('Ctrl Pts',(35.6555077526845,51.562500006828,-35.6555077526845));
#18737=CARTESIAN_POINT('Ctrl Pts',(42.1809185638422,51.3541666734946,-24.3531646875));
#18738=CARTESIAN_POINT('Ctrl Pts',(48.706329375,51.1458333401613,-13.0508216223155));
#18739=CARTESIAN_POINT('Ctrl Pts',(48.706329375,50.937500006828,1.293339198242E-14));
#18740=CARTESIAN_POINT('Ctrl Pts',(48.706329375,50.7291666734946,13.0508216223155));
#18741=CARTESIAN_POINT('Ctrl Pts',(42.1809185638422,50.5208333401613,24.3531646875));
#18742=CARTESIAN_POINT('Ctrl Pts',(35.6555077526845,50.312500006828,35.6555077526845));
#18743=CARTESIAN_POINT('Ctrl Pts',(24.3531646875,50.1041666734946,42.1809185638422));
#18744=CARTESIAN_POINT('Ctrl Pts',(13.0508216223155,49.8958333401613,48.706329375));
#18745=CARTESIAN_POINT('Ctrl Pts',(-9.95098946405443E-15,49.687500006828,
48.706329375));
#18746=CARTESIAN_POINT('Ctrl Pts',(-13.0508216223155,49.4791666734946,48.706329375));
#18747=CARTESIAN_POINT('Ctrl Pts',(-24.3531646875,49.2708333401613,42.1809185638423));
#18748=CARTESIAN_POINT('Ctrl Pts',(-35.6555077526845,49.062500006828,35.6555077526845));
#18749=CARTESIAN_POINT('Ctrl Pts',(-42.1809185638422,48.8541666734946,24.3531646875));
#18750=CARTESIAN_POINT('Ctrl Pts',(-48.706329375,48.6458333401613,13.0508216223155));
#18751=CARTESIAN_POINT('Ctrl Pts',(-48.706329375,48.437500006828,-1.8898197019151E-14));
#18752=CARTESIAN_POINT('Ctrl Pts',(-48.706329375,48.2291666734946,-13.0508216223155));
#18753=CARTESIAN_POINT('Ctrl Pts',(-42.1809185638422,48.0208333401613,-24.3531646875));
#18754=CARTESIAN_POINT('Ctrl Pts',(-35.6555077526845,47.812500006828,-35.6555077526845));
#18755=CARTESIAN_POINT('Ctrl Pts',(-24.3531646875,47.6041666734946,-42.1809185638422));
#18756=CARTESIAN_POINT('Ctrl Pts',(-13.0508216223155,47.3958333401613,-48.706329375));
#18757=CARTESIAN_POINT('Ctrl Pts',(1.59157945007855E-14,47.187500006828,
-48.706329375));
#18758=CARTESIAN_POINT('Ctrl Pts',(13.0508216223155,46.9791666734946,-48.706329375));
#18759=CARTESIAN_POINT('Ctrl Pts',(24.3531646875,46.7708333401613,-42.1809185638422));
#18760=CARTESIAN_POINT('Ctrl Pts',(35.6555077526845,46.562500006828,-35.6555077526845));
#18761=CARTESIAN_POINT('Ctrl Pts',(42.1809185638422,46.3541666734946,-24.3531646875));
#18762=CARTESIAN_POINT('Ctrl Pts',(48.706329375,46.1458333401613,-13.0508216223155));
#18763=CARTESIAN_POINT('Ctrl Pts',(48.706329375,45.937500006828,1.293339198242E-14));
#18764=CARTESIAN_POINT('Ctrl Pts',(48.706329375,45.7291666734946,13.0508216223155));
#18765=CARTESIAN_POINT('Ctrl Pts',(42.1809185638422,45.5208333401613,24.3531646875));
#18766=CARTESIAN_POINT('Ctrl Pts',(35.6555077526845,45.312500006828,35.6555077526845));
#18767=CARTESIAN_POINT('Ctrl Pts',(24.3531646875,45.1041666734946,42.1809185638422));
#18768=CARTESIAN_POINT('Ctrl Pts',(13.0508216223155,44.8958333401613,48.706329375));
#18769=CARTESIAN_POINT('Ctrl Pts',(-9.95098946405443E-15,44.687500006828,
48.706329375));
#18770=CARTESIAN_POINT('Ctrl Pts',(-13.0508216223155,44.4791666734946,48.706329375));
#18771=CARTESIAN_POINT('Ctrl Pts',(-24.3531646875,44.2708333401613,42.1809185638423));
#18772=CARTESIAN_POINT('Ctrl Pts',(-35.6555077526845,44.062500006828,35.6555077526845));
#18773=CARTESIAN_POINT('Ctrl Pts',(-42.1809185638422,43.8541666734946,24.3531646875));
#18774=CARTESIAN_POINT('Ctrl Pts',(-48.706329375,43.6458333401613,13.0508216223155));
#18775=CARTESIAN_POINT('Ctrl Pts',(-48.706329375,43.437500006828,-1.8898197019151E-14));
#18776=CARTESIAN_POINT('Ctrl Pts',(-48.706329375,43.2291666734946,-13.0508216223155));
#18777=CARTESIAN_POINT('Ctrl Pts',(-42.1809185638422,43.0208333401613,-24.3531646875));
#18778=CARTESIAN_POINT('Ctrl Pts',(-35.6555077526845,42.812500006828,-35.6555077526845));
#18779=CARTESIAN_POINT('Ctrl Pts',(-24.3531646875,42.6041666734946,-42.1809185638422));
#18780=CARTESIAN_POINT('Ctrl Pts',(-13.0508216223155,42.3958333401613,-48.706329375));
#18781=CARTESIAN_POINT('Ctrl Pts',(1.59157945007855E-14,42.187500006828,
-48.706329375));
#18782=CARTESIAN_POINT('Ctrl Pts',(13.0508216223155,41.9791666734946,-48.706329375));
#18783=CARTESIAN_POINT('Ctrl Pts',(24.3531646875,41.7708333401613,-42.1809185638422));
#18784=CARTESIAN_POINT('Ctrl Pts',(35.6555077526845,41.562500006828,-35.6555077526845));
#18785=CARTESIAN_POINT('Ctrl Pts',(42.1809185638422,41.3541666734946,-24.3531646875));
#18786=CARTESIAN_POINT('Ctrl Pts',(48.706329375,41.1458333401613,-13.0508216223155));
#18787=CARTESIAN_POINT('Ctrl Pts',(48.706329375,40.937500006828,1.293339198242E-14));
#18788=CARTESIAN_POINT('Ctrl Pts',(48.706329375,40.7291666734946,13.0508216223155));
#18789=CARTESIAN_POINT('Ctrl Pts',(42.1809185638422,40.5208333401613,24.3531646875));
#18790=CARTESIAN_POINT('Ctrl Pts',(35.6555077526845,40.312500006828,35.6555077526845));
#18791=CARTESIAN_POINT('Ctrl Pts',(24.3531646875,40.1041666734946,42.1809185638422));
#18792=CARTESIAN_POINT('Ctrl Pts',(13.0508216223155,39.8958333401613,48.706329375));
#18793=CARTESIAN_POINT('Ctrl Pts',(-9.95098946405443E-15,39.687500006828,
48.706329375));
#18794=CARTESIAN_POINT('Ctrl Pts',(-13.0508216223155,39.4791666734946,48.706329375));
#18795=CARTESIAN_POINT('Ctrl Pts',(-24.3531646875,39.2708333401613,42.1809185638423));
#18796=CARTESIAN_POINT('Ctrl Pts',(-35.6555077526845,39.062500006828,35.6555077526845));
#18797=CARTESIAN_POINT('Ctrl Pts',(-42.1809185638422,38.8541666734946,24.3531646875));
#18798=CARTESIAN_POINT('Ctrl Pts',(-48.706329375,38.6458333401613,13.0508216223155));
#18799=CARTESIAN_POINT('Ctrl Pts',(-48.706329375,38.437500006828,-1.8898197019151E-14));
#18800=CARTESIAN_POINT('Ctrl Pts',(-48.706329375,38.2291666734946,-13.0508216223155));
#18801=CARTESIAN_POINT('Ctrl Pts',(-42.1809185638422,38.0208333401613,-24.3531646875));
#18802=CARTESIAN_POINT('Ctrl Pts',(-35.6555077526845,37.812500006828,-35.6555077526845));
#18803=CARTESIAN_POINT('Ctrl Pts',(-24.3531646875,37.6041666734946,-42.1809185638422));
#18804=CARTESIAN_POINT('Ctrl Pts',(-13.0508216223155,37.3958333401613,-48.706329375));
#18805=CARTESIAN_POINT('Ctrl Pts',(1.59157945007855E-14,37.187500006828,
-48.706329375));
#18806=CARTESIAN_POINT('Ctrl Pts',(13.0508216223155,36.9791666734946,-48.706329375));
#18807=CARTESIAN_POINT('Ctrl Pts',(24.3531646875,36.7708333401613,-42.1809185638422));
#18808=CARTESIAN_POINT('Ctrl Pts',(35.6555077526845,36.562500006828,-35.6555077526845));
#18809=CARTESIAN_POINT('Ctrl Pts',(42.1809185638422,36.3541666734946,-24.3531646875));
#18810=CARTESIAN_POINT('Ctrl Pts',(48.706329375,36.1458333401613,-13.0508216223155));
#18811=CARTESIAN_POINT('Ctrl Pts',(48.706329375,35.937500006828,1.293339198242E-14));
#18812=CARTESIAN_POINT('Ctrl Pts',(48.706329375,35.7291666734946,13.0508216223155));
#18813=CARTESIAN_POINT('Ctrl Pts',(42.1809185638422,35.5208333401613,24.3531646875));
#18814=CARTESIAN_POINT('Ctrl Pts',(35.6555077526845,35.312500006828,35.6555077526845));
#18815=CARTESIAN_POINT('Ctrl Pts',(24.3531646875,35.1041666734946,42.1809185638422));
#18816=CARTESIAN_POINT('Ctrl Pts',(13.0508216223155,34.8958333401613,48.706329375));
#18817=CARTESIAN_POINT('Ctrl Pts',(-9.95098946405443E-15,34.687500006828,
48.706329375));
#18818=CARTESIAN_POINT('Ctrl Pts',(-13.0508216223155,34.4791666734946,48.706329375));
#18819=CARTESIAN_POINT('Ctrl Pts',(-24.3531646875,34.2708333401613,42.1809185638423));
#18820=CARTESIAN_POINT('Ctrl Pts',(-35.6555077526845,34.062500006828,35.6555077526845));
#18821=CARTESIAN_POINT('Ctrl Pts',(-42.1809185638422,33.8541666734946,24.3531646875));
#18822=CARTESIAN_POINT('Ctrl Pts',(-48.706329375,33.6458333401613,13.0508216223155));
#18823=CARTESIAN_POINT('Ctrl Pts',(-48.706329375,33.437500006828,-1.8898197019151E-14));
#18824=CARTESIAN_POINT('Ctrl Pts',(-48.706329375,33.2291666734946,-13.0508216223155));
#18825=CARTESIAN_POINT('Ctrl Pts',(-42.1809185638422,33.0208333401613,-24.3531646875));
#18826=CARTESIAN_POINT('Ctrl Pts',(-35.6555077526845,32.812500006828,-35.6555077526845));
#18827=CARTESIAN_POINT('Ctrl Pts',(-24.3531646875,32.6041666734946,-42.1809185638422));
#18828=CARTESIAN_POINT('Ctrl Pts',(-13.0508216223155,32.3958333401613,-48.706329375));
#18829=CARTESIAN_POINT('Ctrl Pts',(1.59157945007855E-14,32.187500006828,
-48.706329375));
#18830=CARTESIAN_POINT('Ctrl Pts',(13.0508216223155,31.9791666734946,-48.706329375));
#18831=CARTESIAN_POINT('Ctrl Pts',(24.3531646875,31.7708333401613,-42.1809185638422));
#18832=CARTESIAN_POINT('Ctrl Pts',(35.6555077526845,31.562500006828,-35.6555077526845));
#18833=CARTESIAN_POINT('Ctrl Pts',(42.1809185638422,31.3541666734946,-24.3531646875));
#18834=CARTESIAN_POINT('Ctrl Pts',(48.706329375,31.1458333401613,-13.0508216223155));
#18835=CARTESIAN_POINT('Ctrl Pts',(48.706329375,30.937500006828,1.293339198242E-14));
#18836=CARTESIAN_POINT('Ctrl Pts',(48.706329375,30.7291666734946,13.0508216223155));
#18837=CARTESIAN_POINT('Ctrl Pts',(42.1809185638422,30.5208333401613,24.3531646875));
#18838=CARTESIAN_POINT('Ctrl Pts',(35.6555077526845,30.312500006828,35.6555077526845));
#18839=CARTESIAN_POINT('Ctrl Pts',(24.3531646875,30.1041666734946,42.1809185638422));
#18840=CARTESIAN_POINT('Ctrl Pts',(13.0508216223155,29.8958333401613,48.706329375));
#18841=CARTESIAN_POINT('Ctrl Pts',(-9.95098946405443E-15,29.687500006828,
48.706329375));
#18842=CARTESIAN_POINT('Ctrl Pts',(-13.0508216223155,29.4791666734946,48.706329375));
#18843=CARTESIAN_POINT('Ctrl Pts',(-24.3531646875,29.2708333401613,42.1809185638423));
#18844=CARTESIAN_POINT('Ctrl Pts',(-35.6555077526845,29.062500006828,35.6555077526845));
#18845=CARTESIAN_POINT('Ctrl Pts',(-42.1809185638422,28.8541666734946,24.3531646875));
#18846=CARTESIAN_POINT('Ctrl Pts',(-48.706329375,28.6458333401613,13.0508216223155));
#18847=CARTESIAN_POINT('Ctrl Pts',(-48.706329375,28.437500006828,-1.8898197019151E-14));
#18848=CARTESIAN_POINT('Ctrl Pts',(-46.,60.,0.));
#18849=CARTESIAN_POINT('Ctrl Pts',(-46.,59.7916666666667,-12.3256628518316));
#18850=CARTESIAN_POINT('Ctrl Pts',(-39.8371685740842,59.5833333333333,-23.));
#18851=CARTESIAN_POINT('Ctrl Pts',(-33.6743371481684,59.375,-33.6743371481684));
#18852=CARTESIAN_POINT('Ctrl Pts',(-23.,59.1666666666667,-39.8371685740842));
#18853=CARTESIAN_POINT('Ctrl Pts',(-12.3256628518317,58.9583333333333,-46.));
#18854=CARTESIAN_POINT('Ctrl Pts',(-2.81668763803891E-15,58.75,-46.));
#18855=CARTESIAN_POINT('Ctrl Pts',(12.3256628518316,58.5416666666667,-46.));
#18856=CARTESIAN_POINT('Ctrl Pts',(23.,58.3333333333333,-39.8371685740842));
#18857=CARTESIAN_POINT('Ctrl Pts',(33.6743371481683,58.125,-33.6743371481684));
#18858=CARTESIAN_POINT('Ctrl Pts',(39.8371685740842,57.9166666666667,-23.));
#18859=CARTESIAN_POINT('Ctrl Pts',(46.,57.7083333333333,-12.3256628518317));
#18860=CARTESIAN_POINT('Ctrl Pts',(46.,57.5,-5.63337527607782E-15));
#18861=CARTESIAN_POINT('Ctrl Pts',(46.,57.2916666666667,12.3256628518316));
#18862=CARTESIAN_POINT('Ctrl Pts',(39.8371685740842,57.0833333333333,23.));
#18863=CARTESIAN_POINT('Ctrl Pts',(33.6743371481684,56.875,33.6743371481683));
#18864=CARTESIAN_POINT('Ctrl Pts',(23.,56.6666666666667,39.8371685740842));
#18865=CARTESIAN_POINT('Ctrl Pts',(12.3256628518317,56.4583333333333,46.));
#18866=CARTESIAN_POINT('Ctrl Pts',(8.45006291411674E-15,56.25,46.));
#18867=CARTESIAN_POINT('Ctrl Pts',(-12.3256628518316,56.0416666666667,46.));
#18868=CARTESIAN_POINT('Ctrl Pts',(-23.,55.8333333333333,39.8371685740842));
#18869=CARTESIAN_POINT('Ctrl Pts',(-33.6743371481683,55.625,33.6743371481684));
#18870=CARTESIAN_POINT('Ctrl Pts',(-39.8371685740842,55.4166666666667,23.));
#18871=CARTESIAN_POINT('Ctrl Pts',(-46.,55.2083333333333,12.3256628518317));
#18872=CARTESIAN_POINT('Ctrl Pts',(-46.,55.,0.));
#18873=CARTESIAN_POINT('Ctrl Pts',(-46.,54.7916666666667,-12.3256628518316));
#18874=CARTESIAN_POINT('Ctrl Pts',(-39.8371685740842,54.5833333333333,-23.));
#18875=CARTESIAN_POINT('Ctrl Pts',(-33.6743371481684,54.375,-33.6743371481684));
#18876=CARTESIAN_POINT('Ctrl Pts',(-23.,54.1666666666667,-39.8371685740842));
#18877=CARTESIAN_POINT('Ctrl Pts',(-12.3256628518317,53.9583333333333,-46.));
#18878=CARTESIAN_POINT('Ctrl Pts',(-2.81668763803891E-15,53.75,-46.));
#18879=CARTESIAN_POINT('Ctrl Pts',(12.3256628518316,53.5416666666667,-46.));
#18880=CARTESIAN_POINT('Ctrl Pts',(23.,53.3333333333333,-39.8371685740842));
#18881=CARTESIAN_POINT('Ctrl Pts',(33.6743371481683,53.125,-33.6743371481684));
#18882=CARTESIAN_POINT('Ctrl Pts',(39.8371685740842,52.9166666666667,-23.));
#18883=CARTESIAN_POINT('Ctrl Pts',(46.,52.7083333333333,-12.3256628518317));
#18884=CARTESIAN_POINT('Ctrl Pts',(46.,52.5,-5.63337527607782E-15));
#18885=CARTESIAN_POINT('Ctrl Pts',(46.,52.2916666666667,12.3256628518316));
#18886=CARTESIAN_POINT('Ctrl Pts',(39.8371685740842,52.0833333333333,23.));
#18887=CARTESIAN_POINT('Ctrl Pts',(33.6743371481684,51.875,33.6743371481683));
#18888=CARTESIAN_POINT('Ctrl Pts',(23.,51.6666666666667,39.8371685740842));
#18889=CARTESIAN_POINT('Ctrl Pts',(12.3256628518317,51.4583333333333,46.));
#18890=CARTESIAN_POINT('Ctrl Pts',(8.45006291411674E-15,51.25,46.));
#18891=CARTESIAN_POINT('Ctrl Pts',(-12.3256628518316,51.0416666666667,46.));
#18892=CARTESIAN_POINT('Ctrl Pts',(-23.,50.8333333333333,39.8371685740842));
#18893=CARTESIAN_POINT('Ctrl Pts',(-33.6743371481683,50.625,33.6743371481684));
#18894=CARTESIAN_POINT('Ctrl Pts',(-39.8371685740842,50.4166666666667,23.));
#18895=CARTESIAN_POINT('Ctrl Pts',(-46.,50.2083333333333,12.3256628518317));
#18896=CARTESIAN_POINT('Ctrl Pts',(-46.,50.,0.));
#18897=CARTESIAN_POINT('Ctrl Pts',(-46.,49.7916666666667,-12.3256628518316));
#18898=CARTESIAN_POINT('Ctrl Pts',(-39.8371685740842,49.5833333333333,-23.));
#18899=CARTESIAN_POINT('Ctrl Pts',(-33.6743371481684,49.375,-33.6743371481684));
#18900=CARTESIAN_POINT('Ctrl Pts',(-23.,49.1666666666667,-39.8371685740842));
#18901=CARTESIAN_POINT('Ctrl Pts',(-12.3256628518317,48.9583333333333,-46.));
#18902=CARTESIAN_POINT('Ctrl Pts',(-2.81668763803891E-15,48.75,-46.));
#18903=CARTESIAN_POINT('Ctrl Pts',(12.3256628518316,48.5416666666667,-46.));
#18904=CARTESIAN_POINT('Ctrl Pts',(23.,48.3333333333333,-39.8371685740842));
#18905=CARTESIAN_POINT('Ctrl Pts',(33.6743371481683,48.125,-33.6743371481684));
#18906=CARTESIAN_POINT('Ctrl Pts',(39.8371685740842,47.9166666666667,-23.));
#18907=CARTESIAN_POINT('Ctrl Pts',(46.,47.7083333333333,-12.3256628518317));
#18908=CARTESIAN_POINT('Ctrl Pts',(46.,47.5,-5.63337527607782E-15));
#18909=CARTESIAN_POINT('Ctrl Pts',(46.,47.2916666666667,12.3256628518316));
#18910=CARTESIAN_POINT('Ctrl Pts',(39.8371685740842,47.0833333333333,23.));
#18911=CARTESIAN_POINT('Ctrl Pts',(33.6743371481684,46.875,33.6743371481683));
#18912=CARTESIAN_POINT('Ctrl Pts',(23.,46.6666666666667,39.8371685740842));
#18913=CARTESIAN_POINT('Ctrl Pts',(12.3256628518317,46.4583333333333,46.));
#18914=CARTESIAN_POINT('Ctrl Pts',(8.45006291411674E-15,46.25,46.));
#18915=CARTESIAN_POINT('Ctrl Pts',(-12.3256628518316,46.0416666666667,46.));
#18916=CARTESIAN_POINT('Ctrl Pts',(-23.,45.8333333333333,39.8371685740842));
#18917=CARTESIAN_POINT('Ctrl Pts',(-33.6743371481683,45.625,33.6743371481684));
#18918=CARTESIAN_POINT('Ctrl Pts',(-39.8371685740842,45.4166666666667,23.));
#18919=CARTESIAN_POINT('Ctrl Pts',(-46.,45.2083333333333,12.3256628518317));
#18920=CARTESIAN_POINT('Ctrl Pts',(-46.,45.,0.));
#18921=CARTESIAN_POINT('Ctrl Pts',(-46.,44.7916666666667,-12.3256628518316));
#18922=CARTESIAN_POINT('Ctrl Pts',(-39.8371685740842,44.5833333333333,-23.));
#18923=CARTESIAN_POINT('Ctrl Pts',(-33.6743371481684,44.375,-33.6743371481684));
#18924=CARTESIAN_POINT('Ctrl Pts',(-23.,44.1666666666667,-39.8371685740842));
#18925=CARTESIAN_POINT('Ctrl Pts',(-12.3256628518317,43.9583333333333,-46.));
#18926=CARTESIAN_POINT('Ctrl Pts',(-2.81668763803891E-15,43.75,-46.));
#18927=CARTESIAN_POINT('Ctrl Pts',(12.3256628518316,43.5416666666667,-46.));
#18928=CARTESIAN_POINT('Ctrl Pts',(23.,43.3333333333333,-39.8371685740842));
#18929=CARTESIAN_POINT('Ctrl Pts',(33.6743371481683,43.125,-33.6743371481684));
#18930=CARTESIAN_POINT('Ctrl Pts',(39.8371685740842,42.9166666666667,-23.));
#18931=CARTESIAN_POINT('Ctrl Pts',(46.,42.7083333333333,-12.3256628518317));
#18932=CARTESIAN_POINT('Ctrl Pts',(46.,42.5,-5.63337527607782E-15));
#18933=CARTESIAN_POINT('Ctrl Pts',(46.,42.2916666666667,12.3256628518316));
#18934=CARTESIAN_POINT('Ctrl Pts',(39.8371685740842,42.0833333333333,23.));
#18935=CARTESIAN_POINT('Ctrl Pts',(33.6743371481684,41.875,33.6743371481683));
#18936=CARTESIAN_POINT('Ctrl Pts',(23.,41.6666666666667,39.8371685740842));
#18937=CARTESIAN_POINT('Ctrl Pts',(12.3256628518317,41.4583333333333,46.));
#18938=CARTESIAN_POINT('Ctrl Pts',(8.45006291411674E-15,41.25,46.));
#18939=CARTESIAN_POINT('Ctrl Pts',(-12.3256628518316,41.0416666666667,46.));
#18940=CARTESIAN_POINT('Ctrl Pts',(-23.,40.8333333333333,39.8371685740842));
#18941=CARTESIAN_POINT('Ctrl Pts',(-33.6743371481683,40.625,33.6743371481684));
#18942=CARTESIAN_POINT('Ctrl Pts',(-39.8371685740842,40.4166666666667,23.));
#18943=CARTESIAN_POINT('Ctrl Pts',(-46.,40.2083333333333,12.3256628518317));
#18944=CARTESIAN_POINT('Ctrl Pts',(-46.,40.,0.));
#18945=CARTESIAN_POINT('Ctrl Pts',(-46.,39.7916666666667,-12.3256628518316));
#18946=CARTESIAN_POINT('Ctrl Pts',(-39.8371685740842,39.5833333333333,-23.));
#18947=CARTESIAN_POINT('Ctrl Pts',(-33.6743371481684,39.375,-33.6743371481684));
#18948=CARTESIAN_POINT('Ctrl Pts',(-23.,39.1666666666667,-39.8371685740842));
#18949=CARTESIAN_POINT('Ctrl Pts',(-12.3256628518317,38.9583333333333,-46.));
#18950=CARTESIAN_POINT('Ctrl Pts',(-2.81668763803891E-15,38.75,-46.));
#18951=CARTESIAN_POINT('Ctrl Pts',(12.3256628518316,38.5416666666667,-46.));
#18952=CARTESIAN_POINT('Ctrl Pts',(23.,38.3333333333333,-39.8371685740842));
#18953=CARTESIAN_POINT('Ctrl Pts',(33.6743371481683,38.125,-33.6743371481684));
#18954=CARTESIAN_POINT('Ctrl Pts',(39.8371685740842,37.9166666666667,-23.));
#18955=CARTESIAN_POINT('Ctrl Pts',(46.,37.7083333333333,-12.3256628518317));
#18956=CARTESIAN_POINT('Ctrl Pts',(46.,37.5,-5.63337527607782E-15));
#18957=CARTESIAN_POINT('Ctrl Pts',(46.,37.2916666666667,12.3256628518316));
#18958=CARTESIAN_POINT('Ctrl Pts',(39.8371685740842,37.0833333333333,23.));
#18959=CARTESIAN_POINT('Ctrl Pts',(33.6743371481684,36.875,33.6743371481683));
#18960=CARTESIAN_POINT('Ctrl Pts',(23.,36.6666666666667,39.8371685740842));
#18961=CARTESIAN_POINT('Ctrl Pts',(12.3256628518317,36.4583333333333,46.));
#18962=CARTESIAN_POINT('Ctrl Pts',(8.45006291411674E-15,36.25,46.));
#18963=CARTESIAN_POINT('Ctrl Pts',(-12.3256628518316,36.0416666666667,46.));
#18964=CARTESIAN_POINT('Ctrl Pts',(-23.,35.8333333333333,39.8371685740842));
#18965=CARTESIAN_POINT('Ctrl Pts',(-33.6743371481683,35.625,33.6743371481684));
#18966=CARTESIAN_POINT('Ctrl Pts',(-39.8371685740842,35.4166666666667,23.));
#18967=CARTESIAN_POINT('Ctrl Pts',(-46.,35.2083333333333,12.3256628518317));
#18968=CARTESIAN_POINT('Ctrl Pts',(-46.,35.,0.));
#18969=CARTESIAN_POINT('Ctrl Pts',(-46.,34.7916666666667,-12.3256628518316));
#18970=CARTESIAN_POINT('Ctrl Pts',(-39.8371685740842,34.5833333333333,-23.));
#18971=CARTESIAN_POINT('Ctrl Pts',(-33.6743371481684,34.375,-33.6743371481684));
#18972=CARTESIAN_POINT('Ctrl Pts',(-23.,34.1666666666667,-39.8371685740842));
#18973=CARTESIAN_POINT('Ctrl Pts',(-12.3256628518317,33.9583333333333,-46.));
#18974=CARTESIAN_POINT('Ctrl Pts',(-2.81668763803891E-15,33.75,-46.));
#18975=CARTESIAN_POINT('Ctrl Pts',(12.3256628518316,33.5416666666667,-46.));
#18976=CARTESIAN_POINT('Ctrl Pts',(23.,33.3333333333333,-39.8371685740842));
#18977=CARTESIAN_POINT('Ctrl Pts',(33.6743371481683,33.125,-33.6743371481684));
#18978=CARTESIAN_POINT('Ctrl Pts',(39.8371685740842,32.9166666666667,-23.));
#18979=CARTESIAN_POINT('Ctrl Pts',(46.,32.7083333333333,-12.3256628518317));
#18980=CARTESIAN_POINT('Ctrl Pts',(46.,32.5,-5.63337527607782E-15));
#18981=CARTESIAN_POINT('Ctrl Pts',(46.,32.2916666666667,12.3256628518316));
#18982=CARTESIAN_POINT('Ctrl Pts',(39.8371685740842,32.0833333333333,23.));
#18983=CARTESIAN_POINT('Ctrl Pts',(33.6743371481684,31.875,33.6743371481683));
#18984=CARTESIAN_POINT('Ctrl Pts',(23.,31.6666666666667,39.8371685740842));
#18985=CARTESIAN_POINT('Ctrl Pts',(12.3256628518317,31.4583333333333,46.));
#18986=CARTESIAN_POINT('Ctrl Pts',(8.45006291411674E-15,31.25,46.));
#18987=CARTESIAN_POINT('Ctrl Pts',(-12.3256628518316,31.0416666666667,46.));
#18988=CARTESIAN_POINT('Ctrl Pts',(-23.,30.8333333333333,39.8371685740842));
#18989=CARTESIAN_POINT('Ctrl Pts',(-33.6743371481683,30.625,33.6743371481684));
#18990=CARTESIAN_POINT('Ctrl Pts',(-39.8371685740842,30.4166666666667,23.));
#18991=CARTESIAN_POINT('Ctrl Pts',(-46.,30.2083333333333,12.3256628518317));
#18992=CARTESIAN_POINT('Ctrl Pts',(-46.,30.,0.));
#18993=CARTESIAN_POINT('Ctrl Pts',(-45.858362923034,35.061608680256,3.60701400320325));
#18994=CARTESIAN_POINT('Ctrl Pts',(-46.089925771934,34.9280150456296,3.60701400320325));
#18995=CARTESIAN_POINT('Ctrl Pts',(-46.5530501979845,34.6608255719955,3.60701400320344));
#18996=CARTESIAN_POINT('Ctrl Pts',(-47.0161721905706,34.3936318804496,3.60701400320332));
#18997=CARTESIAN_POINT('Ctrl Pts',(-47.6893519862319,34.0052434879083,3.60701400320332));
#18998=CARTESIAN_POINT('Ctrl Pts',(-48.1309692507095,33.7504492807381,3.60701400320324));
#18999=CARTESIAN_POINT('Ctrl Pts',(-48.5725845633798,33.4956516907297,3.60701400320325));
#19000=CARTESIAN_POINT('Ctrl Pts',(-3.5801454378685,34.6297857346188,48.5745723586909));
#19001=CARTESIAN_POINT('Ctrl Pts',(-3.75675791161119,34.8758757672123,48.1282675842178));
#19002=CARTESIAN_POINT('Ctrl Pts',(-3.89802648524866,35.1321260590805,47.6664043022228));
#19003=CARTESIAN_POINT('Ctrl Pts',(-4.11753371733878,35.6479820980819,46.7424335165373));
#19004=CARTESIAN_POINT('Ctrl Pts',(-4.19766087013856,35.9122067971139,46.2720484535312));
#19005=CARTESIAN_POINT('Ctrl Pts',(-4.24983907177926,36.1772764823076,45.8032626333974));
#19006=CARTESIAN_POINT('Ctrl Pts',(-48.706329375,58.437500006828,-1.8898197019151E-14));
#19007=CARTESIAN_POINT('Ctrl Pts',(-48.706329375,58.2291666734946,-13.0508216223155));
#19008=CARTESIAN_POINT('Ctrl Pts',(-42.1809185638422,58.0208333401613,-24.3531646875));
#19009=CARTESIAN_POINT('Ctrl Pts',(-35.6555077526845,57.812500006828,-35.6555077526845));
#19010=CARTESIAN_POINT('Ctrl Pts',(-24.3531646875,57.6041666734946,-42.1809185638422));
#19011=CARTESIAN_POINT('Ctrl Pts',(-13.0508216223155,57.3958333401613,-48.706329375));
#19012=CARTESIAN_POINT('Ctrl Pts',(1.59157945007855E-14,57.187500006828,
-48.706329375));
#19013=CARTESIAN_POINT('Ctrl Pts',(13.0508216223155,56.9791666734946,-48.706329375));
#19014=CARTESIAN_POINT('Ctrl Pts',(24.3531646875,56.7708333401613,-42.1809185638422));
#19015=CARTESIAN_POINT('Ctrl Pts',(35.6555077526845,56.562500006828,-35.6555077526845));
#19016=CARTESIAN_POINT('Ctrl Pts',(42.1809185638422,56.3541666734946,-24.3531646875));
#19017=CARTESIAN_POINT('Ctrl Pts',(48.706329375,56.1458333401613,-13.0508216223155));
#19018=CARTESIAN_POINT('Ctrl Pts',(48.706329375,55.937500006828,1.293339198242E-14));
#19019=CARTESIAN_POINT('Ctrl Pts',(48.706329375,55.7291666734946,13.0508216223155));
#19020=CARTESIAN_POINT('Ctrl Pts',(42.1809185638422,55.5208333401613,24.3531646875));
#19021=CARTESIAN_POINT('Ctrl Pts',(35.6555077526845,55.312500006828,35.6555077526845));
#19022=CARTESIAN_POINT('Ctrl Pts',(24.3531646875,55.1041666734946,42.1809185638422));
#19023=CARTESIAN_POINT('Ctrl Pts',(13.0508216223155,54.8958333401613,48.706329375));
#19024=CARTESIAN_POINT('Ctrl Pts',(-9.95098946405443E-15,54.687500006828,
48.706329375));
#19025=CARTESIAN_POINT('Ctrl Pts',(-13.0508216223155,54.4791666734946,48.706329375));
#19026=CARTESIAN_POINT('Ctrl Pts',(-24.3531646875,54.2708333401613,42.1809185638423));
#19027=CARTESIAN_POINT('Ctrl Pts',(-35.6555077526845,54.062500006828,35.6555077526845));
#19028=CARTESIAN_POINT('Ctrl Pts',(-42.1809185638422,53.8541666734946,24.3531646875));
#19029=CARTESIAN_POINT('Ctrl Pts',(-48.706329375,53.6458333401613,13.0508216223155));
#19030=CARTESIAN_POINT('Ctrl Pts',(-48.706329375,53.437500006828,-1.8898197019151E-14));
#19031=CARTESIAN_POINT('Ctrl Pts',(-48.706329375,53.2291666734946,-13.0508216223155));
#19032=CARTESIAN_POINT('Ctrl Pts',(-42.1809185638422,53.0208333401613,-24.3531646875));
#19033=CARTESIAN_POINT('Ctrl Pts',(-35.6555077526845,52.812500006828,-35.6555077526845));
#19034=CARTESIAN_POINT('Ctrl Pts',(-24.3531646875,52.6041666734946,-42.1809185638422));
#19035=CARTESIAN_POINT('Ctrl Pts',(-13.0508216223155,52.3958333401613,-48.706329375));
#19036=CARTESIAN_POINT('Ctrl Pts',(1.59157945007855E-14,52.187500006828,
-48.706329375));
#19037=CARTESIAN_POINT('Ctrl Pts',(13.0508216223155,51.9791666734946,-48.706329375));
#19038=CARTESIAN_POINT('Ctrl Pts',(24.3531646875,51.7708333401613,-42.1809185638422));
#19039=CARTESIAN_POINT('Ctrl Pts',(35.6555077526845,51.562500006828,-35.6555077526845));
#19040=CARTESIAN_POINT('Ctrl Pts',(42.1809185638422,51.3541666734946,-24.3531646875));
#19041=CARTESIAN_POINT('Ctrl Pts',(48.706329375,51.1458333401613,-13.0508216223155));
#19042=CARTESIAN_POINT('Ctrl Pts',(48.706329375,50.937500006828,1.293339198242E-14));
#19043=CARTESIAN_POINT('Ctrl Pts',(48.706329375,50.7291666734946,13.0508216223155));
#19044=CARTESIAN_POINT('Ctrl Pts',(42.1809185638422,50.5208333401613,24.3531646875));
#19045=CARTESIAN_POINT('Ctrl Pts',(35.6555077526845,50.312500006828,35.6555077526845));
#19046=CARTESIAN_POINT('Ctrl Pts',(24.3531646875,50.1041666734946,42.1809185638422));
#19047=CARTESIAN_POINT('Ctrl Pts',(13.0508216223155,49.8958333401613,48.706329375));
#19048=CARTESIAN_POINT('Ctrl Pts',(-9.95098946405443E-15,49.687500006828,
48.706329375));
#19049=CARTESIAN_POINT('Ctrl Pts',(-13.0508216223155,49.4791666734946,48.706329375));
#19050=CARTESIAN_POINT('Ctrl Pts',(-24.3531646875,49.2708333401613,42.1809185638423));
#19051=CARTESIAN_POINT('Ctrl Pts',(-35.6555077526845,49.062500006828,35.6555077526845));
#19052=CARTESIAN_POINT('Ctrl Pts',(-42.1809185638422,48.8541666734946,24.3531646875));
#19053=CARTESIAN_POINT('Ctrl Pts',(-48.706329375,48.6458333401613,13.0508216223155));
#19054=CARTESIAN_POINT('Ctrl Pts',(-48.706329375,48.437500006828,-1.8898197019151E-14));
#19055=CARTESIAN_POINT('Ctrl Pts',(-48.706329375,48.2291666734946,-13.0508216223155));
#19056=CARTESIAN_POINT('Ctrl Pts',(-42.1809185638422,48.0208333401613,-24.3531646875));
#19057=CARTESIAN_POINT('Ctrl Pts',(-35.6555077526845,47.812500006828,-35.6555077526845));
#19058=CARTESIAN_POINT('Ctrl Pts',(-24.3531646875,47.6041666734946,-42.1809185638422));
#19059=CARTESIAN_POINT('Ctrl Pts',(-13.0508216223155,47.3958333401613,-48.706329375));
#19060=CARTESIAN_POINT('Ctrl Pts',(1.59157945007855E-14,47.187500006828,
-48.706329375));
#19061=CARTESIAN_POINT('Ctrl Pts',(13.0508216223155,46.9791666734946,-48.706329375));
#19062=CARTESIAN_POINT('Ctrl Pts',(24.3531646875,46.7708333401613,-42.1809185638422));
#19063=CARTESIAN_POINT('Ctrl Pts',(35.6555077526845,46.562500006828,-35.6555077526845));
#19064=CARTESIAN_POINT('Ctrl Pts',(42.1809185638422,46.3541666734946,-24.3531646875));
#19065=CARTESIAN_POINT('Ctrl Pts',(48.706329375,46.1458333401613,-13.0508216223155));
#19066=CARTESIAN_POINT('Ctrl Pts',(48.706329375,45.937500006828,1.293339198242E-14));
#19067=CARTESIAN_POINT('Ctrl Pts',(48.706329375,45.7291666734946,13.0508216223155));
#19068=CARTESIAN_POINT('Ctrl Pts',(42.1809185638422,45.5208333401613,24.3531646875));
#19069=CARTESIAN_POINT('Ctrl Pts',(35.6555077526845,45.312500006828,35.6555077526845));
#19070=CARTESIAN_POINT('Ctrl Pts',(24.3531646875,45.1041666734946,42.1809185638422));
#19071=CARTESIAN_POINT('Ctrl Pts',(13.0508216223155,44.8958333401613,48.706329375));
#19072=CARTESIAN_POINT('Ctrl Pts',(-9.95098946405443E-15,44.687500006828,
48.706329375));
#19073=CARTESIAN_POINT('Ctrl Pts',(-13.0508216223155,44.4791666734946,48.706329375));
#19074=CARTESIAN_POINT('Ctrl Pts',(-24.3531646875,44.2708333401613,42.1809185638423));
#19075=CARTESIAN_POINT('Ctrl Pts',(-35.6555077526845,44.062500006828,35.6555077526845));
#19076=CARTESIAN_POINT('Ctrl Pts',(-42.1809185638422,43.8541666734946,24.3531646875));
#19077=CARTESIAN_POINT('Ctrl Pts',(-48.706329375,43.6458333401613,13.0508216223155));
#19078=CARTESIAN_POINT('Ctrl Pts',(-48.706329375,43.437500006828,-1.8898197019151E-14));
#19079=CARTESIAN_POINT('Ctrl Pts',(-48.706329375,43.2291666734946,-13.0508216223155));
#19080=CARTESIAN_POINT('Ctrl Pts',(-42.1809185638422,43.0208333401613,-24.3531646875));
#19081=CARTESIAN_POINT('Ctrl Pts',(-35.6555077526845,42.812500006828,-35.6555077526845));
#19082=CARTESIAN_POINT('Ctrl Pts',(-24.3531646875,42.6041666734946,-42.1809185638422));
#19083=CARTESIAN_POINT('Ctrl Pts',(-13.0508216223155,42.3958333401613,-48.706329375));
#19084=CARTESIAN_POINT('Ctrl Pts',(1.59157945007855E-14,42.187500006828,
-48.706329375));
#19085=CARTESIAN_POINT('Ctrl Pts',(13.0508216223155,41.9791666734946,-48.706329375));
#19086=CARTESIAN_POINT('Ctrl Pts',(24.3531646875,41.7708333401613,-42.1809185638422));
#19087=CARTESIAN_POINT('Ctrl Pts',(35.6555077526845,41.562500006828,-35.6555077526845));
#19088=CARTESIAN_POINT('Ctrl Pts',(42.1809185638422,41.3541666734946,-24.3531646875));
#19089=CARTESIAN_POINT('Ctrl Pts',(48.706329375,41.1458333401613,-13.0508216223155));
#19090=CARTESIAN_POINT('Ctrl Pts',(48.706329375,40.937500006828,1.293339198242E-14));
#19091=CARTESIAN_POINT('Ctrl Pts',(48.706329375,40.7291666734946,13.0508216223155));
#19092=CARTESIAN_POINT('Ctrl Pts',(42.1809185638422,40.5208333401613,24.3531646875));
#19093=CARTESIAN_POINT('Ctrl Pts',(35.6555077526845,40.312500006828,35.6555077526845));
#19094=CARTESIAN_POINT('Ctrl Pts',(24.3531646875,40.1041666734946,42.1809185638422));
#19095=CARTESIAN_POINT('Ctrl Pts',(13.0508216223155,39.8958333401613,48.706329375));
#19096=CARTESIAN_POINT('Ctrl Pts',(-9.95098946405443E-15,39.687500006828,
48.706329375));
#19097=CARTESIAN_POINT('Ctrl Pts',(-13.0508216223155,39.4791666734946,48.706329375));
#19098=CARTESIAN_POINT('Ctrl Pts',(-24.3531646875,39.2708333401613,42.1809185638423));
#19099=CARTESIAN_POINT('Ctrl Pts',(-35.6555077526845,39.062500006828,35.6555077526845));
#19100=CARTESIAN_POINT('Ctrl Pts',(-42.1809185638422,38.8541666734946,24.3531646875));
#19101=CARTESIAN_POINT('Ctrl Pts',(-48.706329375,38.6458333401613,13.0508216223155));
#19102=CARTESIAN_POINT('Ctrl Pts',(-48.706329375,38.437500006828,-1.8898197019151E-14));
#19103=CARTESIAN_POINT('Ctrl Pts',(-48.706329375,38.2291666734946,-13.0508216223155));
#19104=CARTESIAN_POINT('Ctrl Pts',(-42.1809185638422,38.0208333401613,-24.3531646875));
#19105=CARTESIAN_POINT('Ctrl Pts',(-35.6555077526845,37.812500006828,-35.6555077526845));
#19106=CARTESIAN_POINT('Ctrl Pts',(-24.3531646875,37.6041666734946,-42.1809185638422));
#19107=CARTESIAN_POINT('Ctrl Pts',(-13.0508216223155,37.3958333401613,-48.706329375));
#19108=CARTESIAN_POINT('Ctrl Pts',(1.59157945007855E-14,37.187500006828,
-48.706329375));
#19109=CARTESIAN_POINT('Ctrl Pts',(13.0508216223155,36.9791666734946,-48.706329375));
#19110=CARTESIAN_POINT('Ctrl Pts',(24.3531646875,36.7708333401613,-42.1809185638422));
#19111=CARTESIAN_POINT('Ctrl Pts',(35.6555077526845,36.562500006828,-35.6555077526845));
#19112=CARTESIAN_POINT('Ctrl Pts',(42.1809185638422,36.3541666734946,-24.3531646875));
#19113=CARTESIAN_POINT('Ctrl Pts',(48.706329375,36.1458333401613,-13.0508216223155));
#19114=CARTESIAN_POINT('Ctrl Pts',(48.706329375,35.937500006828,1.293339198242E-14));
#19115=CARTESIAN_POINT('Ctrl Pts',(48.706329375,35.7291666734946,13.0508216223155));
#19116=CARTESIAN_POINT('Ctrl Pts',(42.1809185638422,35.5208333401613,24.3531646875));
#19117=CARTESIAN_POINT('Ctrl Pts',(35.6555077526845,35.312500006828,35.6555077526845));
#19118=CARTESIAN_POINT('Ctrl Pts',(24.3531646875,35.1041666734946,42.1809185638422));
#19119=CARTESIAN_POINT('Ctrl Pts',(13.0508216223155,34.8958333401613,48.706329375));
#19120=CARTESIAN_POINT('Ctrl Pts',(-9.95098946405443E-15,34.687500006828,
48.706329375));
#19121=CARTESIAN_POINT('Ctrl Pts',(-13.0508216223155,34.4791666734946,48.706329375));
#19122=CARTESIAN_POINT('Ctrl Pts',(-24.3531646875,34.2708333401613,42.1809185638423));
#19123=CARTESIAN_POINT('Ctrl Pts',(-35.6555077526845,34.062500006828,35.6555077526845));
#19124=CARTESIAN_POINT('Ctrl Pts',(-42.1809185638422,33.8541666734946,24.3531646875));
#19125=CARTESIAN_POINT('Ctrl Pts',(-48.706329375,33.6458333401613,13.0508216223155));
#19126=CARTESIAN_POINT('Ctrl Pts',(-48.706329375,33.437500006828,-1.8898197019151E-14));
#19127=CARTESIAN_POINT('Ctrl Pts',(-48.706329375,33.2291666734946,-13.0508216223155));
#19128=CARTESIAN_POINT('Ctrl Pts',(-42.1809185638422,33.0208333401613,-24.3531646875));
#19129=CARTESIAN_POINT('Ctrl Pts',(-35.6555077526845,32.812500006828,-35.6555077526845));
#19130=CARTESIAN_POINT('Ctrl Pts',(-24.3531646875,32.6041666734946,-42.1809185638422));
#19131=CARTESIAN_POINT('Ctrl Pts',(-13.0508216223155,32.3958333401613,-48.706329375));
#19132=CARTESIAN_POINT('Ctrl Pts',(1.59157945007855E-14,32.187500006828,
-48.706329375));
#19133=CARTESIAN_POINT('Ctrl Pts',(13.0508216223155,31.9791666734946,-48.706329375));
#19134=CARTESIAN_POINT('Ctrl Pts',(24.3531646875,31.7708333401613,-42.1809185638422));
#19135=CARTESIAN_POINT('Ctrl Pts',(35.6555077526845,31.562500006828,-35.6555077526845));
#19136=CARTESIAN_POINT('Ctrl Pts',(42.1809185638422,31.3541666734946,-24.3531646875));
#19137=CARTESIAN_POINT('Ctrl Pts',(48.706329375,31.1458333401613,-13.0508216223155));
#19138=CARTESIAN_POINT('Ctrl Pts',(48.706329375,30.937500006828,1.293339198242E-14));
#19139=CARTESIAN_POINT('Ctrl Pts',(48.706329375,30.7291666734946,13.0508216223155));
#19140=CARTESIAN_POINT('Ctrl Pts',(42.1809185638422,30.5208333401613,24.3531646875));
#19141=CARTESIAN_POINT('Ctrl Pts',(35.6555077526845,30.312500006828,35.6555077526845));
#19142=CARTESIAN_POINT('Ctrl Pts',(24.3531646875,30.1041666734946,42.1809185638422));
#19143=CARTESIAN_POINT('Ctrl Pts',(13.0508216223155,29.8958333401613,48.706329375));
#19144=CARTESIAN_POINT('Ctrl Pts',(-9.95098946405443E-15,29.687500006828,
48.706329375));
#19145=CARTESIAN_POINT('Ctrl Pts',(-13.0508216223155,29.4791666734946,48.706329375));
#19146=CARTESIAN_POINT('Ctrl Pts',(-24.3531646875,29.2708333401613,42.1809185638423));
#19147=CARTESIAN_POINT('Ctrl Pts',(-35.6555077526845,29.062500006828,35.6555077526845));
#19148=CARTESIAN_POINT('Ctrl Pts',(-42.1809185638422,28.8541666734946,24.3531646875));
#19149=CARTESIAN_POINT('Ctrl Pts',(-48.706329375,28.6458333401613,13.0508216223155));
#19150=CARTESIAN_POINT('Ctrl Pts',(-48.706329375,28.437500006828,-1.8898197019151E-14));
#19151=CARTESIAN_POINT('Ctrl Pts',(-46.,60.,0.));
#19152=CARTESIAN_POINT('Ctrl Pts',(-46.,59.7916666666667,-12.3256628518316));
#19153=CARTESIAN_POINT('Ctrl Pts',(-39.8371685740842,59.5833333333333,-23.));
#19154=CARTESIAN_POINT('Ctrl Pts',(-33.6743371481684,59.375,-33.6743371481684));
#19155=CARTESIAN_POINT('Ctrl Pts',(-23.,59.1666666666667,-39.8371685740842));
#19156=CARTESIAN_POINT('Ctrl Pts',(-12.3256628518317,58.9583333333333,-46.));
#19157=CARTESIAN_POINT('Ctrl Pts',(-2.81668763803891E-15,58.75,-46.));
#19158=CARTESIAN_POINT('Ctrl Pts',(12.3256628518316,58.5416666666667,-46.));
#19159=CARTESIAN_POINT('Ctrl Pts',(23.,58.3333333333333,-39.8371685740842));
#19160=CARTESIAN_POINT('Ctrl Pts',(33.6743371481683,58.125,-33.6743371481684));
#19161=CARTESIAN_POINT('Ctrl Pts',(39.8371685740842,57.9166666666667,-23.));
#19162=CARTESIAN_POINT('Ctrl Pts',(46.,57.7083333333333,-12.3256628518317));
#19163=CARTESIAN_POINT('Ctrl Pts',(46.,57.5,-5.63337527607782E-15));
#19164=CARTESIAN_POINT('Ctrl Pts',(46.,57.2916666666667,12.3256628518316));
#19165=CARTESIAN_POINT('Ctrl Pts',(39.8371685740842,57.0833333333333,23.));
#19166=CARTESIAN_POINT('Ctrl Pts',(33.6743371481684,56.875,33.6743371481683));
#19167=CARTESIAN_POINT('Ctrl Pts',(23.,56.6666666666667,39.8371685740842));
#19168=CARTESIAN_POINT('Ctrl Pts',(12.3256628518317,56.4583333333333,46.));
#19169=CARTESIAN_POINT('Ctrl Pts',(8.45006291411674E-15,56.25,46.));
#19170=CARTESIAN_POINT('Ctrl Pts',(-12.3256628518316,56.0416666666667,46.));
#19171=CARTESIAN_POINT('Ctrl Pts',(-23.,55.8333333333333,39.8371685740842));
#19172=CARTESIAN_POINT('Ctrl Pts',(-33.6743371481683,55.625,33.6743371481684));
#19173=CARTESIAN_POINT('Ctrl Pts',(-39.8371685740842,55.4166666666667,23.));
#19174=CARTESIAN_POINT('Ctrl Pts',(-46.,55.2083333333333,12.3256628518317));
#19175=CARTESIAN_POINT('Ctrl Pts',(-46.,55.,0.));
#19176=CARTESIAN_POINT('Ctrl Pts',(-46.,54.7916666666667,-12.3256628518316));
#19177=CARTESIAN_POINT('Ctrl Pts',(-39.8371685740842,54.5833333333333,-23.));
#19178=CARTESIAN_POINT('Ctrl Pts',(-33.6743371481684,54.375,-33.6743371481684));
#19179=CARTESIAN_POINT('Ctrl Pts',(-23.,54.1666666666667,-39.8371685740842));
#19180=CARTESIAN_POINT('Ctrl Pts',(-12.3256628518317,53.9583333333333,-46.));
#19181=CARTESIAN_POINT('Ctrl Pts',(-2.81668763803891E-15,53.75,-46.));
#19182=CARTESIAN_POINT('Ctrl Pts',(12.3256628518316,53.5416666666667,-46.));
#19183=CARTESIAN_POINT('Ctrl Pts',(23.,53.3333333333333,-39.8371685740842));
#19184=CARTESIAN_POINT('Ctrl Pts',(33.6743371481683,53.125,-33.6743371481684));
#19185=CARTESIAN_POINT('Ctrl Pts',(39.8371685740842,52.9166666666667,-23.));
#19186=CARTESIAN_POINT('Ctrl Pts',(46.,52.7083333333333,-12.3256628518317));
#19187=CARTESIAN_POINT('Ctrl Pts',(46.,52.5,-5.63337527607782E-15));
#19188=CARTESIAN_POINT('Ctrl Pts',(46.,52.2916666666667,12.3256628518316));
#19189=CARTESIAN_POINT('Ctrl Pts',(39.8371685740842,52.0833333333333,23.));
#19190=CARTESIAN_POINT('Ctrl Pts',(33.6743371481684,51.875,33.6743371481683));
#19191=CARTESIAN_POINT('Ctrl Pts',(23.,51.6666666666667,39.8371685740842));
#19192=CARTESIAN_POINT('Ctrl Pts',(12.3256628518317,51.4583333333333,46.));
#19193=CARTESIAN_POINT('Ctrl Pts',(8.45006291411674E-15,51.25,46.));
#19194=CARTESIAN_POINT('Ctrl Pts',(-12.3256628518316,51.0416666666667,46.));
#19195=CARTESIAN_POINT('Ctrl Pts',(-23.,50.8333333333333,39.8371685740842));
#19196=CARTESIAN_POINT('Ctrl Pts',(-33.6743371481683,50.625,33.6743371481684));
#19197=CARTESIAN_POINT('Ctrl Pts',(-39.8371685740842,50.4166666666667,23.));
#19198=CARTESIAN_POINT('Ctrl Pts',(-46.,50.2083333333333,12.3256628518317));
#19199=CARTESIAN_POINT('Ctrl Pts',(-46.,50.,0.));
#19200=CARTESIAN_POINT('Ctrl Pts',(-46.,49.7916666666667,-12.3256628518316));
#19201=CARTESIAN_POINT('Ctrl Pts',(-39.8371685740842,49.5833333333333,-23.));
#19202=CARTESIAN_POINT('Ctrl Pts',(-33.6743371481684,49.375,-33.6743371481684));
#19203=CARTESIAN_POINT('Ctrl Pts',(-23.,49.1666666666667,-39.8371685740842));
#19204=CARTESIAN_POINT('Ctrl Pts',(-12.3256628518317,48.9583333333333,-46.));
#19205=CARTESIAN_POINT('Ctrl Pts',(-2.81668763803891E-15,48.75,-46.));
#19206=CARTESIAN_POINT('Ctrl Pts',(12.3256628518316,48.5416666666667,-46.));
#19207=CARTESIAN_POINT('Ctrl Pts',(23.,48.3333333333333,-39.8371685740842));
#19208=CARTESIAN_POINT('Ctrl Pts',(33.6743371481683,48.125,-33.6743371481684));
#19209=CARTESIAN_POINT('Ctrl Pts',(39.8371685740842,47.9166666666667,-23.));
#19210=CARTESIAN_POINT('Ctrl Pts',(46.,47.7083333333333,-12.3256628518317));
#19211=CARTESIAN_POINT('Ctrl Pts',(46.,47.5,-5.63337527607782E-15));
#19212=CARTESIAN_POINT('Ctrl Pts',(46.,47.2916666666667,12.3256628518316));
#19213=CARTESIAN_POINT('Ctrl Pts',(39.8371685740842,47.0833333333333,23.));
#19214=CARTESIAN_POINT('Ctrl Pts',(33.6743371481684,46.875,33.6743371481683));
#19215=CARTESIAN_POINT('Ctrl Pts',(23.,46.6666666666667,39.8371685740842));
#19216=CARTESIAN_POINT('Ctrl Pts',(12.3256628518317,46.4583333333333,46.));
#19217=CARTESIAN_POINT('Ctrl Pts',(8.45006291411674E-15,46.25,46.));
#19218=CARTESIAN_POINT('Ctrl Pts',(-12.3256628518316,46.0416666666667,46.));
#19219=CARTESIAN_POINT('Ctrl Pts',(-23.,45.8333333333333,39.8371685740842));
#19220=CARTESIAN_POINT('Ctrl Pts',(-33.6743371481683,45.625,33.6743371481684));
#19221=CARTESIAN_POINT('Ctrl Pts',(-39.8371685740842,45.4166666666667,23.));
#19222=CARTESIAN_POINT('Ctrl Pts',(-46.,45.2083333333333,12.3256628518317));
#19223=CARTESIAN_POINT('Ctrl Pts',(-46.,45.,0.));
#19224=CARTESIAN_POINT('Ctrl Pts',(-46.,44.7916666666667,-12.3256628518316));
#19225=CARTESIAN_POINT('Ctrl Pts',(-39.8371685740842,44.5833333333333,-23.));
#19226=CARTESIAN_POINT('Ctrl Pts',(-33.6743371481684,44.375,-33.6743371481684));
#19227=CARTESIAN_POINT('Ctrl Pts',(-23.,44.1666666666667,-39.8371685740842));
#19228=CARTESIAN_POINT('Ctrl Pts',(-12.3256628518317,43.9583333333333,-46.));
#19229=CARTESIAN_POINT('Ctrl Pts',(-2.81668763803891E-15,43.75,-46.));
#19230=CARTESIAN_POINT('Ctrl Pts',(12.3256628518316,43.5416666666667,-46.));
#19231=CARTESIAN_POINT('Ctrl Pts',(23.,43.3333333333333,-39.8371685740842));
#19232=CARTESIAN_POINT('Ctrl Pts',(33.6743371481683,43.125,-33.6743371481684));
#19233=CARTESIAN_POINT('Ctrl Pts',(39.8371685740842,42.9166666666667,-23.));
#19234=CARTESIAN_POINT('Ctrl Pts',(46.,42.7083333333333,-12.3256628518317));
#19235=CARTESIAN_POINT('Ctrl Pts',(46.,42.5,-5.63337527607782E-15));
#19236=CARTESIAN_POINT('Ctrl Pts',(46.,42.2916666666667,12.3256628518316));
#19237=CARTESIAN_POINT('Ctrl Pts',(39.8371685740842,42.0833333333333,23.));
#19238=CARTESIAN_POINT('Ctrl Pts',(33.6743371481684,41.875,33.6743371481683));
#19239=CARTESIAN_POINT('Ctrl Pts',(23.,41.6666666666667,39.8371685740842));
#19240=CARTESIAN_POINT('Ctrl Pts',(12.3256628518317,41.4583333333333,46.));
#19241=CARTESIAN_POINT('Ctrl Pts',(8.45006291411674E-15,41.25,46.));
#19242=CARTESIAN_POINT('Ctrl Pts',(-12.3256628518316,41.0416666666667,46.));
#19243=CARTESIAN_POINT('Ctrl Pts',(-23.,40.8333333333333,39.8371685740842));
#19244=CARTESIAN_POINT('Ctrl Pts',(-33.6743371481683,40.625,33.6743371481684));
#19245=CARTESIAN_POINT('Ctrl Pts',(-39.8371685740842,40.4166666666667,23.));
#19246=CARTESIAN_POINT('Ctrl Pts',(-46.,40.2083333333333,12.3256628518317));
#19247=CARTESIAN_POINT('Ctrl Pts',(-46.,40.,0.));
#19248=CARTESIAN_POINT('Ctrl Pts',(-46.,39.7916666666667,-12.3256628518316));
#19249=CARTESIAN_POINT('Ctrl Pts',(-39.8371685740842,39.5833333333333,-23.));
#19250=CARTESIAN_POINT('Ctrl Pts',(-33.6743371481684,39.375,-33.6743371481684));
#19251=CARTESIAN_POINT('Ctrl Pts',(-23.,39.1666666666667,-39.8371685740842));
#19252=CARTESIAN_POINT('Ctrl Pts',(-12.3256628518317,38.9583333333333,-46.));
#19253=CARTESIAN_POINT('Ctrl Pts',(-2.81668763803891E-15,38.75,-46.));
#19254=CARTESIAN_POINT('Ctrl Pts',(12.3256628518316,38.5416666666667,-46.));
#19255=CARTESIAN_POINT('Ctrl Pts',(23.,38.3333333333333,-39.8371685740842));
#19256=CARTESIAN_POINT('Ctrl Pts',(33.6743371481683,38.125,-33.6743371481684));
#19257=CARTESIAN_POINT('Ctrl Pts',(39.8371685740842,37.9166666666667,-23.));
#19258=CARTESIAN_POINT('Ctrl Pts',(46.,37.7083333333333,-12.3256628518317));
#19259=CARTESIAN_POINT('Ctrl Pts',(46.,37.5,-5.63337527607782E-15));
#19260=CARTESIAN_POINT('Ctrl Pts',(46.,37.2916666666667,12.3256628518316));
#19261=CARTESIAN_POINT('Ctrl Pts',(39.8371685740842,37.0833333333333,23.));
#19262=CARTESIAN_POINT('Ctrl Pts',(33.6743371481684,36.875,33.6743371481683));
#19263=CARTESIAN_POINT('Ctrl Pts',(23.,36.6666666666667,39.8371685740842));
#19264=CARTESIAN_POINT('Ctrl Pts',(12.3256628518317,36.4583333333333,46.));
#19265=CARTESIAN_POINT('Ctrl Pts',(8.45006291411674E-15,36.25,46.));
#19266=CARTESIAN_POINT('Ctrl Pts',(-12.3256628518316,36.0416666666667,46.));
#19267=CARTESIAN_POINT('Ctrl Pts',(-23.,35.8333333333333,39.8371685740842));
#19268=CARTESIAN_POINT('Ctrl Pts',(-33.6743371481683,35.625,33.6743371481684));
#19269=CARTESIAN_POINT('Ctrl Pts',(-39.8371685740842,35.4166666666667,23.));
#19270=CARTESIAN_POINT('Ctrl Pts',(-46.,35.2083333333333,12.3256628518317));
#19271=CARTESIAN_POINT('Ctrl Pts',(-46.,35.,0.));
#19272=CARTESIAN_POINT('Ctrl Pts',(-46.,34.7916666666667,-12.3256628518316));
#19273=CARTESIAN_POINT('Ctrl Pts',(-39.8371685740842,34.5833333333333,-23.));
#19274=CARTESIAN_POINT('Ctrl Pts',(-33.6743371481684,34.375,-33.6743371481684));
#19275=CARTESIAN_POINT('Ctrl Pts',(-23.,34.1666666666667,-39.8371685740842));
#19276=CARTESIAN_POINT('Ctrl Pts',(-12.3256628518317,33.9583333333333,-46.));
#19277=CARTESIAN_POINT('Ctrl Pts',(-2.81668763803891E-15,33.75,-46.));
#19278=CARTESIAN_POINT('Ctrl Pts',(12.3256628518316,33.5416666666667,-46.));
#19279=CARTESIAN_POINT('Ctrl Pts',(23.,33.3333333333333,-39.8371685740842));
#19280=CARTESIAN_POINT('Ctrl Pts',(33.6743371481683,33.125,-33.6743371481684));
#19281=CARTESIAN_POINT('Ctrl Pts',(39.8371685740842,32.9166666666667,-23.));
#19282=CARTESIAN_POINT('Ctrl Pts',(46.,32.7083333333333,-12.3256628518317));
#19283=CARTESIAN_POINT('Ctrl Pts',(46.,32.5,-5.63337527607782E-15));
#19284=CARTESIAN_POINT('Ctrl Pts',(46.,32.2916666666667,12.3256628518316));
#19285=CARTESIAN_POINT('Ctrl Pts',(39.8371685740842,32.0833333333333,23.));
#19286=CARTESIAN_POINT('Ctrl Pts',(33.6743371481684,31.875,33.6743371481683));
#19287=CARTESIAN_POINT('Ctrl Pts',(23.,31.6666666666667,39.8371685740842));
#19288=CARTESIAN_POINT('Ctrl Pts',(12.3256628518317,31.4583333333333,46.));
#19289=CARTESIAN_POINT('Ctrl Pts',(8.45006291411674E-15,31.25,46.));
#19290=CARTESIAN_POINT('Ctrl Pts',(-12.3256628518316,31.0416666666667,46.));
#19291=CARTESIAN_POINT('Ctrl Pts',(-23.,30.8333333333333,39.8371685740842));
#19292=CARTESIAN_POINT('Ctrl Pts',(-33.6743371481683,30.625,33.6743371481684));
#19293=CARTESIAN_POINT('Ctrl Pts',(-39.8371685740842,30.4166666666667,23.));
#19294=CARTESIAN_POINT('Ctrl Pts',(-46.,30.2083333333333,12.3256628518317));
#19295=CARTESIAN_POINT('Ctrl Pts',(-46.,30.,0.));
#19296=CARTESIAN_POINT('',(-46.6620925223333,29.597913825102,3.60701400320327));
#19297=CARTESIAN_POINT('',(-45.858362923034,30.061608680256,3.60701400320318));
#19298=CARTESIAN_POINT('Ctrl Pts',(-46.6620925223333,29.597913825102,3.60701400320326));
#19299=CARTESIAN_POINT('Ctrl Pts',(-46.9829117922315,29.4128216316687,3.60701400320326));
#19300=CARTESIAN_POINT('Ctrl Pts',(-47.3046963748559,29.2275305610077,3.5940657325934));
#19301=CARTESIAN_POINT('Ctrl Pts',(-47.9453311027174,28.8592841960704,3.54210581887907));
#19302=CARTESIAN_POINT('Ctrl Pts',(-48.2659302181934,28.6753237953703,3.50295023343856));
#19303=CARTESIAN_POINT('Ctrl Pts',(-48.5839797682363,28.4930986521586,3.45013493440412));
#19304=CARTESIAN_POINT('Ctrl Pts',(48.5725845633798,30.8793483229262,3.60701400320327));
#19305=CARTESIAN_POINT('Ctrl Pts',(48.3407853679392,31.0125314497137,3.60701400320327));
#19306=CARTESIAN_POINT('Ctrl Pts',(48.1089821836664,31.1457076343818,3.60701400320325));
#19307=CARTESIAN_POINT('Ctrl Pts',(47.6453674864979,31.4120455056142,3.60701400320325));
#19308=CARTESIAN_POINT('Ctrl Pts',(47.4135559734253,31.5452071923974,3.60701400320323));
#19309=CARTESIAN_POINT('Ctrl Pts',(47.1817401099609,31.6783613050641,3.60701400320323));
#19310=CARTESIAN_POINT('Ctrl Pts',(46.7406305897488,31.9317328641751,3.60701400320323));
#19311=CARTESIAN_POINT('Ctrl Pts',(46.2995053259033,32.1850770165972,3.60701400320323));
#19312=CARTESIAN_POINT('Ctrl Pts',(45.858362923034,32.438391319744,3.60701400320325));
#19313=CARTESIAN_POINT('Origin',(107.751358612144,29.597913825102,-0.361735996796731));
#19314=CARTESIAN_POINT('',(65.,29.597913825102,-4.33048599679673));
#19315=CARTESIAN_POINT('',(107.751358612144,28.,-3.99459271982449));
#19316=CARTESIAN_POINT('',(107.751358612144,28.,3.27112072623103));
#19317=CARTESIAN_POINT('',(65.,29.597913825102,3.60701400320327));
#19318=CARTESIAN_POINT('Origin',(107.751358612144,29.597913825102,-0.361735996796731));
#19319=CARTESIAN_POINT('',(107.751358612144,29.597913825102,-4.33048599679673));
#19320=CARTESIAN_POINT('',(107.751358612144,29.597913825102,3.60701400320327));
#19321=CARTESIAN_POINT('',(45.8835457347666,28.,3.27112072623103));
#19322=CARTESIAN_POINT('Origin',(46.089894195239,29.5885902225026,-0.356468963009084));
#19323=CARTESIAN_POINT('',(107.751358612144,28.,3.27112072623103));
#19324=CARTESIAN_POINT('',(107.751358612144,28.,-3.99459271982449));
#19325=CARTESIAN_POINT('Origin',(0.,60.,0.));
#19326=CARTESIAN_POINT('',(3.61292728433799,60.,45.8578974271399));
#19327=CARTESIAN_POINT('Origin',(0.,57.,0.));
#19328=CARTESIAN_POINT('',(3.61292728433799,57.,-48.4459777332189));
#19329=CARTESIAN_POINT('Origin',(-0.355816377580837,36.9438035983105,109.846845895932));
#19330=CARTESIAN_POINT('',(-4.32456320853981,36.9438035983105,109.846845895932));
#19331=CARTESIAN_POINT('',(3.61293045337858,36.9438035983105,109.846845895932));
#19332=CARTESIAN_POINT('Origin',(0.,60.,0.));
#19333=CARTESIAN_POINT('Origin',(0.,28.,0.));
#19334=CARTESIAN_POINT('Origin',(0.,28.,0.));
#19335=CARTESIAN_POINT('Origin',(0.,28.,0.));
#19336=CARTESIAN_POINT('Origin',(0.,0.,0.));
#19337=CARTESIAN_POINT('Origin',(0.,20.,0.));
#19338=CARTESIAN_POINT('Origin',(-0.355816377580837,36.9438035983105,109.846845895932));
#19339=CARTESIAN_POINT('',(-4.32456320853981,36.9438035983105,109.846845895932));
#19340=CARTESIAN_POINT('',(3.61293045337858,36.9438035983105,109.846845895932));
#19341=CARTESIAN_POINT('Origin',(-4.32456003949879,64.1203831012736,71.));
#19342=CARTESIAN_POINT('Origin',(3.61292728433799,36.9367107508029,71.));
#19343=CARTESIAN_POINT('Origin',(-4.32456003949879,64.1203831012736,71.));
#19344=CARTESIAN_POINT('Origin',(3.61292728433799,36.9367107508029,71.));
#19345=CARTESIAN_POINT('Origin',(65.,29.597913825102,3.60701400320327));
#19346=CARTESIAN_POINT('Origin',(65.,60.4726068567958,-4.33048599679673));
#19347=CARTESIAN_POINT('Origin',(65.,29.597913825102,3.60701400320327));
#19348=CARTESIAN_POINT('Origin',(65.,60.4726068567958,-4.33048599679673));
#19349=CARTESIAN_POINT('Origin',(65.,60.4726068567958,-4.33048599679673));
#19350=CARTESIAN_POINT('Origin',(0.,3.42,0.));
#19351=CARTESIAN_POINT('',(0.,0.,0.));
#19352=CARTESIAN_POINT('Origin',(-4.44089209850063E-14,2.18749999317203,
-8.4502213867173E-14));
#19353=CARTESIAN_POINT('',(-47.293670625,19.062499993172,-2.74087067386922E-14));
#19354=CARTESIAN_POINT('',(-47.293670625,20.312499993172,-2.29764507158874E-14));
#19355=CARTESIAN_POINT('',(-47.2936706250001,2.18749999317203,-1.6342946393376E-13));
#19356=CARTESIAN_POINT('',(-44.6588684919845,20.58,15.5652416043447));
#19357=CARTESIAN_POINT('Ctrl Pts',(-47.293670625,20.312499993172,-4.77048955893622E-15));
#19358=CARTESIAN_POINT('Ctrl Pts',(-47.293670625,20.4441128906546,8.00562351734399));
#19359=CARTESIAN_POINT('Ctrl Pts',(-44.6588684919845,20.58,15.5652416043447));
#19360=CARTESIAN_POINT('',(14.6145423619412,20.58,44.9789554429287));
#19361=CARTESIAN_POINT('Origin',(-4.44089209850065E-14,20.58,3.95490361115957E-14));
#19362=CARTESIAN_POINT('',(14.6145423715095,20.5629604749638,44.9789554528196));
#19363=CARTESIAN_POINT('',(14.6145423672912,20.5629605363188,44.9789554411892));
#19364=CARTESIAN_POINT('Ctrl Pts',(-47.293670625,19.062499993172,-5.20417042793042E-15));
#19365=CARTESIAN_POINT('Ctrl Pts',(-47.293670625,19.2708333265054,12.6723008510722));
#19366=CARTESIAN_POINT('Ctrl Pts',(-40.9575201994638,19.4791666598387,23.6468353125));
#19367=CARTESIAN_POINT('Ctrl Pts',(-34.6213697739277,19.687499993172,34.6213697739277));
#19368=CARTESIAN_POINT('Ctrl Pts',(-23.6468353125,19.8958333265054,40.9575201994639));
#19369=CARTESIAN_POINT('Ctrl Pts',(-12.6723008510723,20.1041666598387,47.293670625));
#19370=CARTESIAN_POINT('Ctrl Pts',(-2.77555756156289E-14,20.312499993172,
47.293670625));
#19371=CARTESIAN_POINT('Ctrl Pts',(7.4905755366668,20.4356454731033,47.293670625));
#19372=CARTESIAN_POINT('Ctrl Pts',(14.6145423683093,20.5629604365775,44.9789554408594));
#19373=CARTESIAN_POINT('Origin',(-4.44089209850063E-14,2.18749999317203,
-8.4502213867173E-14));
#19374=CARTESIAN_POINT('',(-47.293670625,14.062499993172,-4.42703690919226E-14));
#19375=CARTESIAN_POINT('',(-47.293670625,15.312499993172,-3.98381130691179E-14));
#19376=CARTESIAN_POINT('',(-47.2936706250001,2.18749999317203,-1.6342946393376E-13));
#19377=CARTESIAN_POINT('Ctrl Pts',(-47.293670625,15.312499993172,-4.77048955893622E-15));
#19378=CARTESIAN_POINT('Ctrl Pts',(-47.293670625,15.5208333265054,12.6723008510722));
#19379=CARTESIAN_POINT('Ctrl Pts',(-40.9575201994638,15.7291666598387,23.6468353125));
#19380=CARTESIAN_POINT('Ctrl Pts',(-34.6213697739277,15.937499993172,34.6213697739277));
#19381=CARTESIAN_POINT('Ctrl Pts',(-23.6468353125,16.1458333265054,40.9575201994638));
#19382=CARTESIAN_POINT('Ctrl Pts',(-12.6723008510723,16.3541666598387,47.293670625));
#19383=CARTESIAN_POINT('Ctrl Pts',(-2.77555756156289E-14,16.562499993172,
47.293670625));
#19384=CARTESIAN_POINT('Ctrl Pts',(12.6723008510722,16.7708333265054,47.293670625));
#19385=CARTESIAN_POINT('Ctrl Pts',(23.6468353125,16.9791666598387,40.9575201994639));
#19386=CARTESIAN_POINT('Ctrl Pts',(34.6213697739277,17.187499993172,34.6213697739278));
#19387=CARTESIAN_POINT('Ctrl Pts',(40.9575201994639,17.3958333265054,23.6468353125));
#19388=CARTESIAN_POINT('Ctrl Pts',(47.293670625,17.6041666598387,12.6723008510723));
#19389=CARTESIAN_POINT('Ctrl Pts',(47.293670625,17.812499993172,4.33680868994202E-16));
#19390=CARTESIAN_POINT('Ctrl Pts',(47.293670625,18.0208333265054,-12.6723008510723));
#19391=CARTESIAN_POINT('Ctrl Pts',(40.9575201994639,18.2291666598387,-23.6468353125));
#19392=CARTESIAN_POINT('Ctrl Pts',(34.6213697739278,18.437499993172,-34.6213697739277));
#19393=CARTESIAN_POINT('Ctrl Pts',(23.6468353125,18.6458333265054,-40.9575201994639));
#19394=CARTESIAN_POINT('Ctrl Pts',(12.6723008510723,18.8541666598387,-47.293670625));
#19395=CARTESIAN_POINT('Ctrl Pts',(0.,19.062499993172,-47.293670625));
#19396=CARTESIAN_POINT('Ctrl Pts',(-12.6723008510723,19.2708333265054,-47.293670625));
#19397=CARTESIAN_POINT('Ctrl Pts',(-23.6468353125,19.4791666598387,-40.9575201994639));
#19398=CARTESIAN_POINT('Ctrl Pts',(-34.6213697739277,19.687499993172,-34.6213697739277));
#19399=CARTESIAN_POINT('Ctrl Pts',(-40.9575201994638,19.8958333265054,-23.6468353125));
#19400=CARTESIAN_POINT('Ctrl Pts',(-47.293670625,20.1041666598387,-12.6723008510723));
#19401=CARTESIAN_POINT('Ctrl Pts',(-47.293670625,20.312499993172,-4.77048955893622E-15));
#19402=CARTESIAN_POINT('Ctrl Pts',(-47.293670625,14.062499993172,-5.20417042793042E-15));
#19403=CARTESIAN_POINT('Ctrl Pts',(-47.293670625,14.2708333265054,12.6723008510722));
#19404=CARTESIAN_POINT('Ctrl Pts',(-40.9575201994638,14.4791666598387,23.6468353125));
#19405=CARTESIAN_POINT('Ctrl Pts',(-34.6213697739277,14.687499993172,34.6213697739277));
#19406=CARTESIAN_POINT('Ctrl Pts',(-23.6468353125,14.8958333265054,40.9575201994639));
#19407=CARTESIAN_POINT('Ctrl Pts',(-12.6723008510723,15.1041666598387,47.293670625));
#19408=CARTESIAN_POINT('Ctrl Pts',(-2.77555756156289E-14,15.312499993172,
47.293670625));
#19409=CARTESIAN_POINT('Ctrl Pts',(12.6723008510722,15.5208333265054,47.293670625));
#19410=CARTESIAN_POINT('Ctrl Pts',(23.6468353125,15.7291666598387,40.9575201994639));
#19411=CARTESIAN_POINT('Ctrl Pts',(34.6213697739277,15.937499993172,34.6213697739278));
#19412=CARTESIAN_POINT('Ctrl Pts',(40.9575201994639,16.1458333265054,23.6468353125));
#19413=CARTESIAN_POINT('Ctrl Pts',(47.293670625,16.3541666598387,12.6723008510723));
#19414=CARTESIAN_POINT('Ctrl Pts',(47.293670625,16.562499993172,0.));
#19415=CARTESIAN_POINT('Ctrl Pts',(47.293670625,16.7708333265054,-12.6723008510723));
#19416=CARTESIAN_POINT('Ctrl Pts',(40.9575201994639,16.9791666598387,-23.6468353125));
#19417=CARTESIAN_POINT('Ctrl Pts',(34.6213697739278,17.187499993172,-34.6213697739277));
#19418=CARTESIAN_POINT('Ctrl Pts',(23.6468353125,17.3958333265054,-40.9575201994639));
#19419=CARTESIAN_POINT('Ctrl Pts',(12.6723008510723,17.6041666598387,-47.293670625));
#19420=CARTESIAN_POINT('Ctrl Pts',(0.,17.812499993172,-47.293670625));
#19421=CARTESIAN_POINT('Ctrl Pts',(-12.6723008510723,18.0208333265054,-47.293670625));
#19422=CARTESIAN_POINT('Ctrl Pts',(-23.6468353125,18.2291666598387,-40.9575201994639));
#19423=CARTESIAN_POINT('Ctrl Pts',(-34.6213697739277,18.437499993172,-34.6213697739278));
#19424=CARTESIAN_POINT('Ctrl Pts',(-40.9575201994638,18.6458333265054,-23.6468353125));
#19425=CARTESIAN_POINT('Ctrl Pts',(-47.293670625,18.8541666598387,-12.6723008510723));
#19426=CARTESIAN_POINT('Ctrl Pts',(-47.293670625,19.062499993172,-5.20417042793042E-15));
#19427=CARTESIAN_POINT('Origin',(-4.44089209850063E-14,2.18749999317203,
-8.4502213867173E-14));
#19428=CARTESIAN_POINT('',(-47.293670625,9.06249999317203,-6.11320314451531E-14));
#19429=CARTESIAN_POINT('',(-47.293670625,10.312499993172,-5.66997754223483E-14));
#19430=CARTESIAN_POINT('',(-47.2936706250001,2.18749999317203,-1.6342946393376E-13));
#19431=CARTESIAN_POINT('Ctrl Pts',(-47.293670625,10.312499993172,-4.77048955893622E-15));
#19432=CARTESIAN_POINT('Ctrl Pts',(-47.293670625,10.5208333265054,12.6723008510722));
#19433=CARTESIAN_POINT('Ctrl Pts',(-40.9575201994638,10.7291666598387,23.6468353125));
#19434=CARTESIAN_POINT('Ctrl Pts',(-34.6213697739277,10.937499993172,34.6213697739277));
#19435=CARTESIAN_POINT('Ctrl Pts',(-23.6468353125,11.1458333265054,40.9575201994638));
#19436=CARTESIAN_POINT('Ctrl Pts',(-12.6723008510723,11.3541666598387,47.293670625));
#19437=CARTESIAN_POINT('Ctrl Pts',(-2.77555756156289E-14,11.562499993172,
47.293670625));
#19438=CARTESIAN_POINT('Ctrl Pts',(12.6723008510722,11.7708333265054,47.293670625));
#19439=CARTESIAN_POINT('Ctrl Pts',(23.6468353125,11.9791666598387,40.9575201994639));
#19440=CARTESIAN_POINT('Ctrl Pts',(34.6213697739277,12.187499993172,34.6213697739278));
#19441=CARTESIAN_POINT('Ctrl Pts',(40.9575201994639,12.3958333265054,23.6468353125));
#19442=CARTESIAN_POINT('Ctrl Pts',(47.293670625,12.6041666598387,12.6723008510723));
#19443=CARTESIAN_POINT('Ctrl Pts',(47.293670625,12.812499993172,4.33680868994202E-16));
#19444=CARTESIAN_POINT('Ctrl Pts',(47.293670625,13.0208333265054,-12.6723008510723));
#19445=CARTESIAN_POINT('Ctrl Pts',(40.9575201994639,13.2291666598387,-23.6468353125));
#19446=CARTESIAN_POINT('Ctrl Pts',(34.6213697739278,13.437499993172,-34.6213697739277));
#19447=CARTESIAN_POINT('Ctrl Pts',(23.6468353125,13.6458333265054,-40.9575201994639));
#19448=CARTESIAN_POINT('Ctrl Pts',(12.6723008510723,13.8541666598387,-47.293670625));
#19449=CARTESIAN_POINT('Ctrl Pts',(0.,14.062499993172,-47.293670625));
#19450=CARTESIAN_POINT('Ctrl Pts',(-12.6723008510723,14.2708333265054,-47.293670625));
#19451=CARTESIAN_POINT('Ctrl Pts',(-23.6468353125,14.4791666598387,-40.9575201994639));
#19452=CARTESIAN_POINT('Ctrl Pts',(-34.6213697739277,14.687499993172,-34.6213697739277));
#19453=CARTESIAN_POINT('Ctrl Pts',(-40.9575201994638,14.8958333265054,-23.6468353125));
#19454=CARTESIAN_POINT('Ctrl Pts',(-47.293670625,15.1041666598387,-12.6723008510723));
#19455=CARTESIAN_POINT('Ctrl Pts',(-47.293670625,15.312499993172,-4.77048955893622E-15));
#19456=CARTESIAN_POINT('Ctrl Pts',(-47.293670625,9.06249999317203,-5.20417042793042E-15));
#19457=CARTESIAN_POINT('Ctrl Pts',(-47.293670625,9.27083332650536,12.6723008510722));
#19458=CARTESIAN_POINT('Ctrl Pts',(-40.9575201994638,9.4791666598387,23.6468353125));
#19459=CARTESIAN_POINT('Ctrl Pts',(-34.6213697739277,9.68749999317203,34.6213697739277));
#19460=CARTESIAN_POINT('Ctrl Pts',(-23.6468353125,9.89583332650536,40.9575201994639));
#19461=CARTESIAN_POINT('Ctrl Pts',(-12.6723008510723,10.1041666598387,47.293670625));
#19462=CARTESIAN_POINT('Ctrl Pts',(-2.77555756156289E-14,10.312499993172,
47.293670625));
#19463=CARTESIAN_POINT('Ctrl Pts',(12.6723008510722,10.5208333265054,47.293670625));
#19464=CARTESIAN_POINT('Ctrl Pts',(23.6468353125,10.7291666598387,40.9575201994639));
#19465=CARTESIAN_POINT('Ctrl Pts',(34.6213697739277,10.937499993172,34.6213697739278));
#19466=CARTESIAN_POINT('Ctrl Pts',(40.9575201994639,11.1458333265054,23.6468353125));
#19467=CARTESIAN_POINT('Ctrl Pts',(47.293670625,11.3541666598387,12.6723008510723));
#19468=CARTESIAN_POINT('Ctrl Pts',(47.293670625,11.562499993172,0.));
#19469=CARTESIAN_POINT('Ctrl Pts',(47.293670625,11.7708333265054,-12.6723008510723));
#19470=CARTESIAN_POINT('Ctrl Pts',(40.9575201994639,11.9791666598387,-23.6468353125));
#19471=CARTESIAN_POINT('Ctrl Pts',(34.6213697739278,12.187499993172,-34.6213697739277));
#19472=CARTESIAN_POINT('Ctrl Pts',(23.6468353125,12.3958333265054,-40.9575201994639));
#19473=CARTESIAN_POINT('Ctrl Pts',(12.6723008510723,12.6041666598387,-47.293670625));
#19474=CARTESIAN_POINT('Ctrl Pts',(0.,12.812499993172,-47.293670625));
#19475=CARTESIAN_POINT('Ctrl Pts',(-12.6723008510723,13.0208333265054,-47.293670625));
#19476=CARTESIAN_POINT('Ctrl Pts',(-23.6468353125,13.2291666598387,-40.9575201994639));
#19477=CARTESIAN_POINT('Ctrl Pts',(-34.6213697739277,13.437499993172,-34.6213697739278));
#19478=CARTESIAN_POINT('Ctrl Pts',(-40.9575201994638,13.6458333265054,-23.6468353125));
#19479=CARTESIAN_POINT('Ctrl Pts',(-47.293670625,13.8541666598387,-12.6723008510723));
#19480=CARTESIAN_POINT('Ctrl Pts',(-47.293670625,14.062499993172,-5.20417042793042E-15));
#19481=CARTESIAN_POINT('Origin',(-4.44089209850063E-14,2.18749999317203,
-8.4502213867173E-14));
#19482=CARTESIAN_POINT('',(-47.293670625,4.06249999317204,-7.79936937983835E-14));
#19483=CARTESIAN_POINT('',(-47.293670625,5.31249999317204,-7.35614377755788E-14));
#19484=CARTESIAN_POINT('',(-47.2936706250001,2.18749999317203,-1.6342946393376E-13));
#19485=CARTESIAN_POINT('',(47.293670625,1.56249999317203,0.));
#19486=CARTESIAN_POINT('Ctrl Pts',(47.293670625,1.56249999317203,0.));
#19487=CARTESIAN_POINT('Ctrl Pts',(47.293670625,1.77083332650536,-12.6723008510723));
#19488=CARTESIAN_POINT('Ctrl Pts',(40.9575201994639,1.9791666598387,-23.6468353125));
#19489=CARTESIAN_POINT('Ctrl Pts',(34.6213697739278,2.18749999317203,-34.6213697739277));
#19490=CARTESIAN_POINT('Ctrl Pts',(23.6468353125,2.39583332650536,-40.9575201994639));
#19491=CARTESIAN_POINT('Ctrl Pts',(12.6723008510723,2.6041666598387,-47.293670625));
#19492=CARTESIAN_POINT('Ctrl Pts',(0.,2.81249999317203,-47.293670625));
#19493=CARTESIAN_POINT('Ctrl Pts',(-12.6723008510723,3.02083332650537,-47.293670625));
#19494=CARTESIAN_POINT('Ctrl Pts',(-23.6468353125,3.2291666598387,-40.9575201994639));
#19495=CARTESIAN_POINT('Ctrl Pts',(-34.6213697739277,3.43749999317203,-34.6213697739278));
#19496=CARTESIAN_POINT('Ctrl Pts',(-40.9575201994638,3.64583332650537,-23.6468353125));
#19497=CARTESIAN_POINT('Ctrl Pts',(-47.293670625,3.8541666598387,-12.6723008510723));
#19498=CARTESIAN_POINT('Ctrl Pts',(-47.293670625,4.06249999317204,-5.20417042793042E-15));
#19499=CARTESIAN_POINT('',(47.293670625,2.81249999317203,4.33680868994202E-16));
#19500=CARTESIAN_POINT('',(47.293670625,2.81249999317203,4.33680868994202E-16));
#19501=CARTESIAN_POINT('Ctrl Pts',(47.293670625,2.81249999317203,4.33680868994202E-16));
#19502=CARTESIAN_POINT('Ctrl Pts',(47.293670625,3.02083332650537,-12.6723008510723));
#19503=CARTESIAN_POINT('Ctrl Pts',(40.9575201994639,3.2291666598387,-23.6468353125));
#19504=CARTESIAN_POINT('Ctrl Pts',(34.6213697739278,3.43749999317203,-34.6213697739277));
#19505=CARTESIAN_POINT('Ctrl Pts',(23.6468353125,3.64583332650537,-40.9575201994639));
#19506=CARTESIAN_POINT('Ctrl Pts',(12.6723008510723,3.8541666598387,-47.293670625));
#19507=CARTESIAN_POINT('Ctrl Pts',(0.,4.06249999317204,-47.293670625));
#19508=CARTESIAN_POINT('Ctrl Pts',(-12.6723008510723,4.27083332650536,-47.293670625));
#19509=CARTESIAN_POINT('Ctrl Pts',(-23.6468353125,4.4791666598387,-40.9575201994639));
#19510=CARTESIAN_POINT('Ctrl Pts',(-34.6213697739277,4.68749999317204,-34.6213697739277));
#19511=CARTESIAN_POINT('Ctrl Pts',(-40.9575201994638,4.89583332650537,-23.6468353125));
#19512=CARTESIAN_POINT('Ctrl Pts',(-47.293670625,5.1041666598387,-12.6723008510723));
#19513=CARTESIAN_POINT('Ctrl Pts',(-47.293670625,5.31249999317204,-4.77048955893622E-15));
#19514=CARTESIAN_POINT('Origin',(0.,30.,0.));
#19515=CARTESIAN_POINT('',(-3.61672851018096E-15,3.75,50.));
#19516=CARTESIAN_POINT('',(-6.12323399573677E-15,0.,50.));
#19517=CARTESIAN_POINT('',(-6.12323399573677E-15,30.,50.));
#19518=CARTESIAN_POINT('',(50.,0.,4.33680868994202E-16));
#19519=CARTESIAN_POINT('Origin',(0.,0.,0.));
#19520=CARTESIAN_POINT('Ctrl Pts',(50.,1.06165076729781E-14,-2.22044604925031E-15));
#19521=CARTESIAN_POINT('Ctrl Pts',(50.,0.0675815458886919,-4.34602095458794));
#19522=CARTESIAN_POINT('Ctrl Pts',(49.433363177975,0.137236267109327,-8.67353338775704));
#19523=CARTESIAN_POINT('Ctrl Pts',(47.1953230212392,0.277178851018911,-17.0732528980021));
#19524=CARTESIAN_POINT('Ctrl Pts',(45.5332330036253,0.346871852511727,-21.1097012523794));
#19525=CARTESIAN_POINT('Ctrl Pts',(40.1317492627809,0.515793945868729,-30.5253872857993));
#19526=CARTESIAN_POINT('Ctrl Pts',(35.8219475848477,0.621158082158269,-35.4844500978245));
#19527=CARTESIAN_POINT('Ctrl Pts',(25.5795028430515,0.828373107047328,-43.4450365132807));
#19528=CARTESIAN_POINT('Ctrl Pts',(19.7547036395998,0.927746124936861,-46.3846276563406));
#19529=CARTESIAN_POINT('Ctrl Pts',(7.27375715639306,1.1364474793245,-49.8934263074991));
#19530=CARTESIAN_POINT('Ctrl Pts',(0.731992466642528,1.2368859786089,-50.4155320575528));
#19531=CARTESIAN_POINT('Ctrl Pts',(-12.2694666320475,1.4453065174627,-48.9167086614796));
#19532=CARTESIAN_POINT('Ctrl Pts',(-18.5997310439367,1.55224307809009,-46.8768025214219));
#19533=CARTESIAN_POINT('Ctrl Pts',(-30.0299904422847,1.75654526614157,-40.5025862073931));
#19534=CARTESIAN_POINT('Ctrl Pts',(-35.036045408383,1.86107507457517,-36.2592957566779));
#19535=CARTESIAN_POINT('Ctrl Pts',(-43.120111853279,2.06848140107261,-26.1235259446925));
#19536=CARTESIAN_POINT('Ctrl Pts',(-46.1326953039639,2.16765558228902,-20.3360992301171));
#19537=CARTESIAN_POINT('Ctrl Pts',(-49.8001432688674,2.37642657857554,-7.89318418467289));
#19538=CARTESIAN_POINT('Ctrl Pts',(-50.403689005381,2.47731150480502,-1.35087920859845));
#19539=CARTESIAN_POINT('Ctrl Pts',(-49.0628121307921,2.68532756322191,11.6668902834284));
#19540=CARTESIAN_POINT('Ctrl Pts',(-47.1039105257039,2.79218578597068,18.0138220579311));
#19541=CARTESIAN_POINT('Ctrl Pts',(-40.881726186314,2.99688303055821,29.5102235202591));
#19542=CARTESIAN_POINT('Ctrl Pts',(-36.7076021277602,3.10060669623969,34.5647456017332));
#19543=CARTESIAN_POINT('Ctrl Pts',(-26.6829381859637,3.30819972311771,42.7763188165426));
#19544=CARTESIAN_POINT('Ctrl Pts',(-20.9345141514266,3.40723200021609,45.8643504967883));
#19545=CARTESIAN_POINT('Ctrl Pts',(-9.96972190006956,3.59185030232342,49.2515812260447));
#19546=CARTESIAN_POINT('Ctrl Pts',(-4.99455109538804,3.67233367312923,50.));
#19547=CARTESIAN_POINT('Ctrl Pts',(1.11022302462516E-15,3.75000000000001,
50.));
#19548=CARTESIAN_POINT('Origin',(0.,30.,0.));
#19549=CARTESIAN_POINT('',(-1.63842932933703E-14,8.75,50.));
#19550=CARTESIAN_POINT('',(2.8024627691636E-14,8.12499998634407,50.));
#19551=CARTESIAN_POINT('',(-6.12323399573677E-15,30.,50.));
#19552=CARTESIAN_POINT('',(50.,4.37499998634407,4.33680868994202E-16));
#19553=CARTESIAN_POINT('Ctrl Pts',(3.77475828372553E-14,8.12499998634407,
50.));
#19554=CARTESIAN_POINT('Ctrl Pts',(-6.29656683951167,8.02708703901777,50.));
#19555=CARTESIAN_POINT('Ctrl Pts',(-12.5395378026787,7.92505148761976,48.8105524892163));
#19556=CARTESIAN_POINT('Ctrl Pts',(-24.428748973416,7.72056704948577,44.1054274881654));
#19557=CARTESIAN_POINT('Ctrl Pts',(-29.9370959070449,7.62102578272423,40.568739744262));
#19558=CARTESIAN_POINT('Ctrl Pts',(-39.2829518076402,7.4125611305386,31.6017896070106));
#19559=CARTESIAN_POINT('Ctrl Pts',(-43.036824942223,7.31238179776275,26.2612876234044));
#19560=CARTESIAN_POINT('Ctrl Pts',(-48.3273553137792,7.10574897519395,14.3907774590969));
#19561=CARTESIAN_POINT('Ctrl Pts',(-49.791594591191,6.99971009509526,7.96399144170724));
#19562=CARTESIAN_POINT('Ctrl Pts',(-50.1681486104848,6.79458070879849,-5.12653202942374));
#19563=CARTESIAN_POINT('Ctrl Pts',(-49.0619331605251,6.68971160553214,-11.6641350292155));
#19564=CARTESIAN_POINT('Ctrl Pts',(-44.4171209681097,6.48077343574223,-23.8559166804422));
#19565=CARTESIAN_POINT('Ctrl Pts',(-40.9550834065452,6.38147848262782,-29.4052106806457));
#19566=CARTESIAN_POINT('Ctrl Pts',(-32.113466366765,6.17312980425173,-38.8662118322004));
#19567=CARTESIAN_POINT('Ctrl Pts',(-26.820282375283,6.07251482308326,-42.6910956804875));
#19568=CARTESIAN_POINT('Ctrl Pts',(-15.009584552541,5.86615268861856,-48.1398836046983));
#19569=CARTESIAN_POINT('Ctrl Pts',(-8.59369004350663,5.75993421526962,-49.6878729247248));
#19570=CARTESIAN_POINT('Ctrl Pts',(4.48774492525712,5.55426543933499,-50.2277992097));
#19571=CARTESIAN_POINT('Ctrl Pts',(11.0271640436078,5.45022299225461,-49.2074578926806));
#19572=CARTESIAN_POINT('Ctrl Pts',(23.2638995025692,5.24128050504109,-44.729379413062));
#19573=CARTESIAN_POINT('Ctrl Pts',(28.8548134450474,5.14217116635957,-41.3439967022577));
#19574=CARTESIAN_POINT('Ctrl Pts',(38.433121503277,4.93395386608903,-32.6312276229427));
#19575=CARTESIAN_POINT('Ctrl Pts',(42.3304633933119,4.83282603182798,-27.3867424586433));
#19576=CARTESIAN_POINT('Ctrl Pts',(46.7247122573551,4.67141859868476,-18.1844199659609));
#19577=CARTESIAN_POINT('Ctrl Pts',(47.949072379614,4.61142813276804,-14.6546310169365));
#19578=CARTESIAN_POINT('Ctrl Pts',(49.5874843271383,4.49186567045974,-7.404842522204));
#19579=CARTESIAN_POINT('Ctrl Pts',(50.,4.43266281444172,-3.7081699732958));
#19580=CARTESIAN_POINT('Ctrl Pts',(50.,4.37499998634406,-1.11022302462516E-15));
#19581=CARTESIAN_POINT('',(50.,2.18749999317203,4.33680868994202E-16));
#19582=CARTESIAN_POINT('Origin',(0.,0.,0.));
#19583=CARTESIAN_POINT('Ctrl Pts',(-1.38777878078145E-15,3.75000000000001,
50.));
#19584=CARTESIAN_POINT('Ctrl Pts',(1.50002951166462,3.77332577645995,50.));
#19585=CARTESIAN_POINT('Ctrl Pts',(3.00179837118478,3.79695985428445,49.9324990070492));
#19586=CARTESIAN_POINT('Ctrl Pts',(11.0440849325066,3.9250477770621,49.2056195962975));
#19587=CARTESIAN_POINT('Ctrl Pts',(17.4071452363091,4.0318085869817,47.3302895610126));
#19588=CARTESIAN_POINT('Ctrl Pts',(28.9703187695284,4.23689013305346,41.2650696264942));
#19589=CARTESIAN_POINT('Ctrl Pts',(34.0743240006798,4.33984944424209,37.162163128162));
#19590=CARTESIAN_POINT('Ctrl Pts',(42.4162332551277,4.54762178810859,27.2520829284582));
#19591=CARTESIAN_POINT('Ctrl Pts',(45.5814688037948,4.64657621006581,21.5439667179538));
#19592=CARTESIAN_POINT('Ctrl Pts',(49.5807884827107,4.85545523193025,9.18302954234058));
#19593=CARTESIAN_POINT('Ctrl Pts',(50.3548312508471,4.95745741831768,2.64074335025333));
#19594=CARTESIAN_POINT('Ctrl Pts',(49.3431424035077,5.16456855488943,-10.4070382692032));
#19595=CARTESIAN_POINT('Ctrl Pts',(47.5531367195831,5.27121261121499,-16.7854529965516));
#19596=CARTESIAN_POINT('Ctrl Pts',(41.6483204537289,5.47666231002944,-28.4152816584745));
#19597=CARTESIAN_POINT('Ctrl Pts',(37.6180020049751,5.57891128315246,-33.5692881184128));
#19598=CARTESIAN_POINT('Ctrl Pts',(27.8249007712785,5.78685301485799,-42.0430563993917));
#19599=CARTESIAN_POINT('Ctrl Pts',(22.1580244614444,5.88579837872905,-45.286483980451));
#19600=CARTESIAN_POINT('Ctrl Pts',(9.8403808718465,6.09471262938967,-49.4558324330969));
#19601=CARTESIAN_POINT('Ctrl Pts',(3.2987214372498,6.19738209975368,-50.3173000552676));
#19602=CARTESIAN_POINT('Ctrl Pts',(-9.76230561520494,6.40399928058008,-49.4735932157222));
#19603=CARTESIAN_POINT('Ctrl Pts',(-16.155095216762,6.51050773208155,-47.7697804504798));
#19604=CARTESIAN_POINT('Ctrl Pts',(-27.8507188284245,6.7163046564155,-42.0271801552601));
#19605=CARTESIAN_POINT('Ctrl Pts',(-33.0547271997935,6.81790741632008,-38.0700878384781));
#19606=CARTESIAN_POINT('Ctrl Pts',(-41.6605133560118,7.02600643206108,-28.3951876913978));
#19607=CARTESIAN_POINT('Ctrl Pts',(-44.9823163989605,7.12501350110592,-22.7700748235208));
#19608=CARTESIAN_POINT('Ctrl Pts',(-49.3221121430825,7.33394910022637,-10.4967295754095));
#19609=CARTESIAN_POINT('Ctrl Pts',(-50.2712713321659,7.43735106074952,-3.95612890853374));
#19610=CARTESIAN_POINT('Ctrl Pts',(-49.5954802301861,7.64345278002998,9.11674282900515));
#19611=CARTESIAN_POINT('Ctrl Pts',(-47.9778112005811,7.74980803904956,15.5227631025264));
#19612=CARTESIAN_POINT('Ctrl Pts',(-42.3975433426475,7.95592734940999,27.2826154977726));
#19613=CARTESIAN_POINT('Ctrl Pts',(-38.5135601479802,8.05695543575843,32.5361107635385));
#19614=CARTESIAN_POINT('Ctrl Pts',(-28.9568652006334,8.26519795013379,41.2727079144305));
#19615=CARTESIAN_POINT('Ctrl Pts',(-23.3736122913173,8.36433646334925,44.6722598314387));
#19616=CARTESIAN_POINT('Ctrl Pts',(-11.7545603061111,8.5628659464166,48.9564434230258));
#19617=CARTESIAN_POINT('Ctrl Pts',(-5.89770451089775,8.65828944632209,50.));
#19618=CARTESIAN_POINT('Ctrl Pts',(-7.7715611723761E-15,8.75,50.));
#19619=CARTESIAN_POINT('Origin',(0.,30.,0.));
#19620=CARTESIAN_POINT('',(-2.42252434047854E-14,13.75,50.));
#19621=CARTESIAN_POINT('',(-4.17184002249354E-15,13.1249999863441,50.));
#19622=CARTESIAN_POINT('',(-6.12323399573677E-15,30.,50.));
#19623=CARTESIAN_POINT('Ctrl Pts',(-5.96744875736022E-15,13.1249999863441,
50.));
#19624=CARTESIAN_POINT('Ctrl Pts',(-0.612619827520453,13.1154736183356,
50.));
#19625=CARTESIAN_POINT('Ctrl Pts',(-1.22568533661716,13.1058934073382,49.9887409889087));
#19626=CARTESIAN_POINT('Ctrl Pts',(-8.36880293377376,12.99372105772,49.7258548775597));
#19627=CARTESIAN_POINT('Ctrl Pts',(-14.7887116767695,12.8875648584764,48.2077926679319));
#19628=CARTESIAN_POINT('Ctrl Pts',(-26.6209452131421,12.6811033461879,42.8155264434361));
#19629=CARTESIAN_POINT('Ctrl Pts',(-31.9310851228465,12.5806516520033,39.0160191601527));
#19630=CARTESIAN_POINT('Ctrl Pts',(-40.8057542169951,12.3725378273868,29.6087010491045));
#19631=CARTESIAN_POINT('Ctrl Pts',(-44.2878907791481,12.2734177967731,24.0908202803128));
#19632=CARTESIAN_POINT('Ctrl Pts',(-48.9708157369014,12.0659484255844,12.0037061295532));
#19633=CARTESIAN_POINT('Ctrl Pts',(-50.1147724065617,11.9616918437045,5.54420998717902));
#19634=CARTESIAN_POINT('Ctrl Pts',(-49.8654311432801,11.7572567880282,-7.5357491602242));
#19635=CARTESIAN_POINT('Ctrl Pts',(-48.4409462355628,11.6503443297974,-14.0293652220786));
#19636=CARTESIAN_POINT('Ctrl Pts',(-43.1903182014914,11.4420551877761,-26.0170814558177));
#19637=CARTESIAN_POINT('Ctrl Pts',(-39.4439086950383,11.341475742409,-31.408120562985));
#19638=CARTESIAN_POINT('Ctrl Pts',(-30.1256355899705,11.1327501431137,-40.4255766808516));
#19639=CARTESIAN_POINT('Ctrl Pts',(-24.6527667112495,11.0334493868274,-43.9775217975006));
#19640=CARTESIAN_POINT('Ctrl Pts',(-12.6197365300443,10.8261700974901,-48.8166712331727));
#19641=CARTESIAN_POINT('Ctrl Pts',(-6.16767509119308,10.7210870421483,-50.0428165881525));
#19642=CARTESIAN_POINT('Ctrl Pts',(6.92971901291009,10.5170510432878,-49.9543171048813));
#19643=CARTESIAN_POINT('Ctrl Pts',(13.4481566577371,10.4100724633252,-48.6065983903204));
#19644=CARTESIAN_POINT('Ctrl Pts',(25.498360373273,10.2014016282185,-43.4975704726577));
#19645=CARTESIAN_POINT('Ctrl Pts',(30.9283498624805,10.1012198621366,-39.8201208804137));
#19646=CARTESIAN_POINT('Ctrl Pts',(40.0546020277859,9.89256933257104,-30.6172384055382));
#19647=CARTESIAN_POINT('Ctrl Pts',(43.6733473464145,9.79303668021819,-25.1878012179268));
#19648=CARTESIAN_POINT('Ctrl Pts',(48.6619829859239,9.58595245791768,-13.2073700775111));
#19649=CARTESIAN_POINT('Ctrl Pts',(49.9668720867691,9.4803009190459,-6.76279537354238));
#19650=CARTESIAN_POINT('Ctrl Pts',(50.0322701358121,9.27625560249255,6.34138794158945));
#19651=CARTESIAN_POINT('Ctrl Pts',(48.7616176208319,9.16964206396107,12.8742939124214));
#19652=CARTESIAN_POINT('Ctrl Pts',(43.7978146143124,8.96075145047578,24.9775439909932));
#19653=CARTESIAN_POINT('Ctrl Pts',(40.1891374783696,8.86091135354223,30.446006767238));
#19654=CARTESIAN_POINT('Ctrl Pts',(31.1014595076989,8.65234622350278,39.6799614216987));
#19655=CARTESIAN_POINT('Ctrl Pts',(25.7154264922144,8.55252643893411,43.3649295856025));
#19656=CARTESIAN_POINT('Ctrl Pts',(13.7882235291873,8.34565299031822,48.5016298032087));
#19657=CARTESIAN_POINT('Ctrl Pts',(7.35188535745777,8.23980419052421,49.884600682187));
#19658=CARTESIAN_POINT('Ctrl Pts',(0.55443206066175,8.13363112474586,49.9976954032747));
#19659=CARTESIAN_POINT('Ctrl Pts',(0.277164254761756,8.12930994918079,50.));
#19660=CARTESIAN_POINT('Ctrl Pts',(3.99680288865056E-14,8.12499998634407,
50.));
#19661=CARTESIAN_POINT('Ctrl Pts',(1.23512311489549E-14,8.75,50.));
#19662=CARTESIAN_POINT('Ctrl Pts',(0.648431293727216,8.7600832438892,50.));
#19663=CARTESIAN_POINT('Ctrl Pts',(1.29735475152641,8.77022669851377,49.9873862048369));
#19664=CARTESIAN_POINT('Ctrl Pts',(8.47721354847014,8.88304048381026,49.7076755550476));
#19665=CARTESIAN_POINT('Ctrl Pts',(14.8952044698391,8.98922696256952,48.1751888538927));
#19666=CARTESIAN_POINT('Ctrl Pts',(26.7170806653891,9.19564094423076,42.7556758577737));
#19667=CARTESIAN_POINT('Ctrl Pts',(32.0190546959999,9.29617028212578,38.9439377316323));
#19668=CARTESIAN_POINT('Ctrl Pts',(40.8728047658779,9.50427955327015,29.5161006010544));
#19669=CARTESIAN_POINT('Ctrl Pts',(44.3424804612446,9.60337391611804,23.9902255380222));
#19670=CARTESIAN_POINT('Ctrl Pts',(48.9975251595022,9.81087599828454,11.89353732302));
#19671=CARTESIAN_POINT('Ctrl Pts',(50.1268184516499,9.9149912031465,5.43274833024308));
#19672=CARTESIAN_POINT('Ctrl Pts',(49.8487676493035,10.119495407801,-7.64396493843533));
#19673=CARTESIAN_POINT('Ctrl Pts',(48.4106012754521,10.2263944461158,-14.1330520571305));
#19674=CARTESIAN_POINT('Ctrl Pts',(43.1347113770559,10.4346133937934,-26.1094853504774));
#19675=CARTESIAN_POINT('Ctrl Pts',(39.375966943307,10.5352697812222,-31.4935174489505));
#19676=CARTESIAN_POINT('Ctrl Pts',(30.0370674477733,10.7440076792621,-40.4914275730604));
#19677=CARTESIAN_POINT('Ctrl Pts',(24.5564395131693,10.8432729235818,-44.0313815757612));
#19678=CARTESIAN_POINT('Ctrl Pts',(12.5140651326065,11.0505856889662,-48.8436922359968));
#19679=CARTESIAN_POINT('Ctrl Pts',(6.06070339202204,11.1555226333687,-50.0557150028884));
#19680=CARTESIAN_POINT('Ctrl Pts',(-7.03378622739985,11.3596285829729,-49.9395876567563));
#19681=CARTESIAN_POINT('Ctrl Pts',(-13.5480267689982,11.4665968972053,-48.5786689149347));
#19682=CARTESIAN_POINT('Ctrl Pts',(-25.587584156021,11.6752035609711,-43.4453094801511));
#19683=CARTESIAN_POINT('Ctrl Pts',(-31.0109196299649,11.775449619827,-39.7560319739043));
#19684=CARTESIAN_POINT('Ctrl Pts',(-40.1185685393079,11.9841137816881,-30.5333486991097));
#19685=CARTESIAN_POINT('Ctrl Pts',(-43.7258848211684,12.0836026544728,-25.0964556960894));
#19686=CARTESIAN_POINT('Ctrl Pts',(-48.6889465030587,12.2907212194005,-13.1069635353675));
#19687=CARTESIAN_POINT('Ctrl Pts',(-49.9803639739704,12.3963372757602,-6.66106092154509));
#19688=CARTESIAN_POINT('Ctrl Pts',(-50.0194334783328,12.6002874467208,6.44405850153165));
#19689=CARTESIAN_POINT('Ctrl Pts',(-48.7348122369756,12.7070587862866,12.9764902577281));
#19690=CARTESIAN_POINT('Ctrl Pts',(-43.7439285895496,12.9159429418896,25.0720688081954));
#19691=CARTESIAN_POINT('Ctrl Pts',(-40.1228032384613,13.0158408141732,30.5335948218922));
#19692=CARTESIAN_POINT('Ctrl Pts',(-31.0142632226721,13.2244221739124,39.748113147005));
#19693=CARTESIAN_POINT('Ctrl Pts',(-25.6203671108846,13.3241858824379,43.4211235514659));
#19694=CARTESIAN_POINT('Ctrl Pts',(-13.6834613648333,13.5310988764741,48.5311033907353));
#19695=CARTESIAN_POINT('Ctrl Pts',(-7.24556749720559,13.6369131113857,49.8999727618044));
#19696=CARTESIAN_POINT('Ctrl Pts',(-0.484352129571248,13.742460893125,49.9982411063084));
#19697=CARTESIAN_POINT('Ctrl Pts',(-0.242136054053174,13.7462347330997,
50.));
#19698=CARTESIAN_POINT('Ctrl Pts',(-2.77555756156289E-16,13.75,50.));
#19699=CARTESIAN_POINT('Origin',(0.,30.,0.));
#19700=CARTESIAN_POINT('',(1.81713983480877E-14,18.75,50.));
#19701=CARTESIAN_POINT('',(-1.31924020975729E-14,18.1249999863441,50.));
#19702=CARTESIAN_POINT('',(-6.12323399573677E-15,30.,50.));
#19703=CARTESIAN_POINT('',(15.4508438171073,19.0004604433872,47.5528277323164));
#19704=CARTESIAN_POINT('Ctrl Pts',(1.66533453693773E-15,18.75,50.));
#19705=CARTESIAN_POINT('Ctrl Pts',(2.06343398963011,18.782086835364,50.));
#19706=CARTESIAN_POINT('Ctrl Pts',(4.12591617046045,18.8146910873865,49.8722678031709));
#19707=CARTESIAN_POINT('Ctrl Pts',(7.74823897426245,18.8728975253031,49.4214154483787));
#19708=CARTESIAN_POINT('Ctrl Pts',(9.31068297651482,18.8983205115452,49.1510191506797));
#19709=CARTESIAN_POINT('Ctrl Pts',(11.6326307868091,18.9365795554256,48.6344758199292));
#19710=CARTESIAN_POINT('Ctrl Pts',(12.4034070010999,18.9493604562429,48.4436356167657));
#19711=CARTESIAN_POINT('Ctrl Pts',(13.5522715319277,18.9685325039609,48.1299649645132));
#19712=CARTESIAN_POINT('Ctrl Pts',(13.9339731925082,18.9749226935498,48.020849453786));
#19713=CARTESIAN_POINT('Ctrl Pts',(14.5044722589624,18.9845043294477,47.8503883399713));
#19714=CARTESIAN_POINT('Ctrl Pts',(14.6942697542235,18.9876971505158,47.792445179082));
#19715=CARTESIAN_POINT('Ctrl Pts',(14.9784245353166,18.9924849931323,47.7038430313957));
#19716=CARTESIAN_POINT('Ctrl Pts',(15.0730437095848,18.9940805597343,47.6740306126352));
#19717=CARTESIAN_POINT('Ctrl Pts',(15.2148336244197,18.9964735029064,47.6288914175082));
#19718=CARTESIAN_POINT('Ctrl Pts',(15.2620713042067,18.9972710408533,47.6137757312423));
#19719=CARTESIAN_POINT('Ctrl Pts',(15.3610459806339,18.9989427577795,47.5819421900349));
#19720=CARTESIAN_POINT('Ctrl Pts',(15.4084466292325,18.9997437594921,47.5666034079044));
#19721=CARTESIAN_POINT('Ctrl Pts',(15.4508438170237,19.0004604433858,47.5528277323436));
#19722=CARTESIAN_POINT('',(15.450843269209,20.58,47.5528279103394));
#19723=CARTESIAN_POINT('',(15.4508436816103,19.3910854416803,47.5528277763422));
#19724=CARTESIAN_POINT('',(2.87173475049016,20.58,-49.9174632721138));
#19725=CARTESIAN_POINT('Origin',(0.,20.58,0.));
#19726=CARTESIAN_POINT('Ctrl Pts',(2.87173475049014,20.58,-49.9174632721138));
#19727=CARTESIAN_POINT('Ctrl Pts',(6.61637351959359,20.5208724585749,-49.7020354723747));
#19728=CARTESIAN_POINT('Ctrl Pts',(10.3248885349788,20.4605538158576,-49.0659276782243));
#19729=CARTESIAN_POINT('Ctrl Pts',(17.5213591482324,20.3399507406698,-46.978783597008));
#19730=CARTESIAN_POINT('Ctrl Pts',(20.9871203622869,20.2800466373442,-45.5361957365975));
#19731=CARTESIAN_POINT('Ctrl Pts',(29.9426187271194,20.1200818557983,-40.5670230702393));
#19732=CARTESIAN_POINT('Ctrl Pts',(34.9568796568864,20.0156924630395,-36.335402485389));
#19733=CARTESIAN_POINT('Ctrl Pts',(43.0625235284044,19.8082537643147,-26.2183663261997));
#19734=CARTESIAN_POINT('Ctrl Pts',(46.0878693059551,19.7091081425281,-20.4375102920327));
#19735=CARTESIAN_POINT('Ctrl Pts',(49.7830590432265,19.5003261545907,-8.00132178314007));
#19736=CARTESIAN_POINT('Ctrl Pts',(50.4008498182792,19.3993573063203,-1.45895842707427));
#19737=CARTESIAN_POINT('Ctrl Pts',(49.0875543111761,19.1914138579732,11.5615320758049));
#19738=CARTESIAN_POINT('Ctrl Pts',(47.1428011004522,19.0845709443303,17.9112704061328));
#19739=CARTESIAN_POINT('Ctrl Pts',(40.9471814385983,18.879806981529,29.419080354316));
#19740=CARTESIAN_POINT('Ctrl Pts',(36.7851237022354,18.7762175138932,34.4820162364731));
#19741=CARTESIAN_POINT('Ctrl Pts',(26.7798605317987,18.5685931862218,42.7157398751768));
#19742=CARTESIAN_POINT('Ctrl Pts',(21.0382551768946,18.4695789482211,45.8168863723286));
#19743=CARTESIAN_POINT('Ctrl Pts',(10.0448695016158,18.2843657945622,49.2401693631193));
#19744=CARTESIAN_POINT('Ctrl Pts',(5.03248290215808,18.2032561608402,50.));
#19745=CARTESIAN_POINT('Ctrl Pts',(-1.11022302462516E-14,18.1249999863441,
50.));
#19746=CARTESIAN_POINT('Origin',(0.,20.58,0.));
#19747=CARTESIAN_POINT('',(-6.4293956955236E-15,20.58,-52.5));
#19748=CARTESIAN_POINT('Origin',(0.,20.58,0.));
#19749=CARTESIAN_POINT('',(-6.4293956955236E-15,23.58,-52.5));
#19750=CARTESIAN_POINT('',(-6.4293956955236E-15,20.58,-52.5));
#19751=CARTESIAN_POINT('Origin',(0.,23.58,0.));
#19752=CARTESIAN_POINT('Origin',(0.,26.58,0.));
#19753=CARTESIAN_POINT('',(-6.4293956955236E-15,26.58,-52.5));
#19754=CARTESIAN_POINT('Origin',(0.,26.58,0.));
#19755=CARTESIAN_POINT('',(-6.4293956955236E-15,30.,-52.5));
#19756=CARTESIAN_POINT('',(-6.4293956955236E-15,26.58,-52.5));
#19757=CARTESIAN_POINT('Origin',(0.,30.,0.));
#19758=CARTESIAN_POINT('Origin',(0.,30.,0.));
#19759=CARTESIAN_POINT('',(-6.85802207522518E-15,0.,56.));
#19760=CARTESIAN_POINT('Origin',(0.,0.,0.));
#19761=CARTESIAN_POINT('',(-6.85802207522518E-15,30.,56.));
#19762=CARTESIAN_POINT('',(-6.85802207522518E-15,30.,56.));
#19763=CARTESIAN_POINT('Origin',(0.,30.,0.));
#19764=CARTESIAN_POINT('Origin',(0.,30.,0.));
#19765=CARTESIAN_POINT('',(-6.12323399573677E-15,26.58,50.));
#19766=CARTESIAN_POINT('Origin',(0.,26.58,0.));
#19767=CARTESIAN_POINT('',(-6.12323399573677E-15,23.58,50.));
#19768=CARTESIAN_POINT('',(-6.12323399573677E-15,30.,50.));
#19769=CARTESIAN_POINT('Origin',(0.,23.58,0.));
#19770=CARTESIAN_POINT('Origin',(0.,30.,0.));
#19771=CARTESIAN_POINT('Ctrl Pts',(0.,18.1249999863441,50.));
#19772=CARTESIAN_POINT('Ctrl Pts',(-1.46395213702768,18.1022352206972,50.));
#19773=CARTESIAN_POINT('Ctrl Pts',(-2.92959655005386,18.079176251773,49.9357068733922));
#19774=CARTESIAN_POINT('Ctrl Pts',(-10.9358446820847,17.9517352605888,49.2295937959252));
#19775=CARTESIAN_POINT('Ctrl Pts',(-17.3015950267471,17.8449930726363,47.3687724018939));
#19776=CARTESIAN_POINT('Ctrl Pts',(-28.8762103510446,17.6398472040909,41.3308164193438));
#19777=CARTESIAN_POINT('Ctrl Pts',(-33.9887542186337,17.5370136598723,37.2402609703136));
#19778=CARTESIAN_POINT('Ctrl Pts',(-42.3531696281848,17.3292115434088,27.3500715192646));
#19779=CARTESIAN_POINT('Ctrl Pts',(-45.5317450789481,17.2302636449031,21.6489612009597));
#19780=CARTESIAN_POINT('Ctrl Pts',(-49.5600708397194,17.0213776385416,9.29534702387663));
#19781=CARTESIAN_POINT('Ctrl Pts',(-50.3490242784998,16.9192661293503,2.75313777136309));
#19782=CARTESIAN_POINT('Ctrl Pts',(-49.3660254411158,16.7122378180411,-10.2970050021595));
#19783=CARTESIAN_POINT('Ctrl Pts',(-47.5907412654829,16.6056156676936,-16.677955620378));
#19784=CARTESIAN_POINT('Ctrl Pts',(-41.7136174652812,16.4001049116793,-28.3191309106804));
#19785=CARTESIAN_POINT('Ctrl Pts',(-37.6958122958252,16.2979713747829,-33.4817130582194));
#19786=CARTESIAN_POINT('Ctrl Pts',(-27.9228961236881,16.0900018004317,-41.9781122685046));
#19787=CARTESIAN_POINT('Ctrl Pts',(-22.2631451216861,15.9910509027763,-45.2349687866989));
#19788=CARTESIAN_POINT('Ctrl Pts',(-9.95302706610038,15.78213199501,-49.4335206200089));
#19789=CARTESIAN_POINT('Ctrl Pts',(-3.41151820394048,15.6793415211135,-50.3100090765765));
#19790=CARTESIAN_POINT('Ctrl Pts',(9.65163979754655,15.472811221036,-49.495106426816));
#19791=CARTESIAN_POINT('Ctrl Pts',(16.0467797762323,15.3663277979795,-47.8060722152372));
#19792=CARTESIAN_POINT('Ctrl Pts',(27.7535304462983,15.1604738188022,-42.0913055049256));
#19793=CARTESIAN_POINT('Ctrl Pts',(32.9660625462325,15.0589746911095,-38.1467601761831));
#19794=CARTESIAN_POINT('Ctrl Pts',(41.5943690684503,14.8508500890501,-28.49213273689));
#19795=CARTESIAN_POINT('Ctrl Pts',(44.929550902591,14.7518253890473,-22.874192221126));
#19796=CARTESIAN_POINT('Ctrl Pts',(49.2984439814791,14.5428875592743,-10.6085001319966));
#19797=CARTESIAN_POINT('Ctrl Pts',(50.2625783652768,14.4393542506304,-4.06812389386595));
#19798=CARTESIAN_POINT('Ctrl Pts',(49.6154032503147,14.2333425384376,9.00662731593866));
#19799=CARTESIAN_POINT('Ctrl Pts',(48.0124121338163,14.1270151373354,15.4147890428637));
#19800=CARTESIAN_POINT('Ctrl Pts',(42.459826826848,13.9208433441612,27.1854340099002));
#19801=CARTESIAN_POINT('Ctrl Pts',(38.5882949974709,13.8199061148943,32.4473144543822));
#19802=CARTESIAN_POINT('Ctrl Pts',(29.0517509449081,13.6116405034011,41.2060914917058));
#19803=CARTESIAN_POINT('Ctrl Pts',(23.4756436865131,13.5124727351935,44.6188352546216));
#19804=CARTESIAN_POINT('Ctrl Pts',(11.8301029936433,13.3133654493466,48.942834310463));
#19805=CARTESIAN_POINT('Ctrl Pts',(5.93604168035801,13.217306691123,50.));
#19806=CARTESIAN_POINT('Ctrl Pts',(-6.66133814775094E-15,13.1249999863441,
50.));
#19807=CARTESIAN_POINT('Ctrl Pts',(-2.66453525910038E-14,13.75,50.));
#19808=CARTESIAN_POINT('Ctrl Pts',(6.33436008535432,13.8485006402999,50.));
#19809=CARTESIAN_POINT('Ctrl Pts',(12.613801309995,13.9511629654864,48.796235648758));
#19810=CARTESIAN_POINT('Ctrl Pts',(24.5279767249908,14.1562049575921,44.0504655224356));
#19811=CARTESIAN_POINT('Ctrl Pts',(30.0291606250117,14.2557956626479,40.5007963959304));
#19812=CARTESIAN_POINT('Ctrl Pts',(39.3549009106075,14.464279263081,31.5120661140904));
#19813=CARTESIAN_POINT('Ctrl Pts',(43.0963799318702,14.5643893391982,26.1633465241914));
#19814=CARTESIAN_POINT('Ctrl Pts',(48.3592590130262,14.7710670457821,14.282540826403));
#19815=CARTESIAN_POINT('Ctrl Pts',(49.8088796826435,14.8770728815201,7.85396277520366));
#19816=CARTESIAN_POINT('Ctrl Pts',(50.1569070724122,15.08210598026,-5.2380123417253));
#19817=CARTESIAN_POINT('Ctrl Pts',(49.0356649182634,15.1871257413067,-11.7752530975039));
#19818=CARTESIAN_POINT('Ctrl Pts',(44.3616870702543,15.3960617215426,-23.9590790294512));
#19819=CARTESIAN_POINT('Ctrl Pts',(40.8862413681065,15.4953961484633,-29.5010488663333));
#19820=CARTESIAN_POINT('Ctrl Pts',(32.0221022500378,15.7037665326716,-38.9414347122342));
#19821=CARTESIAN_POINT('Ctrl Pts',(26.7204115323761,15.8042985976033,-42.7535968627668));
#19822=CARTESIAN_POINT('Ctrl Pts',(14.8988951547692,16.010710919205,-48.1740543034369));
#19823=CARTESIAN_POINT('Ctrl Pts',(8.48097128653307,16.1168984388664,-49.7070410668055));
#19824=CARTESIAN_POINT('Ctrl Pts',(-4.60218838353627,16.322472120921,-50.2177081476848));
#19825=CARTESIAN_POINT('Ctrl Pts',(-11.1413142841139,16.4266580876154,-49.1820099437241));
#19826=CARTESIAN_POINT('Ctrl Pts',(-23.3700742187699,16.6356008217794,-44.6741071340573));
#19827=CARTESIAN_POINT('Ctrl Pts',(-28.9535745488434,16.7347383572907,-41.2750124068013));
#19828=CARTESIAN_POINT('Ctrl Pts',(-38.5109673706576,16.9429800646524,-32.5391840233731));
#19829=CARTESIAN_POINT('Ctrl Pts',(-42.3953818478633,17.0440113346287,-27.2859794219456));
#19830=CARTESIAN_POINT('Ctrl Pts',(-47.976608376972,17.2501288144725,-15.5265016183736));
#19831=CARTESIAN_POINT('Ctrl Pts',(-49.5947857818058,17.3564850292136,-9.12055610322967));
#19832=CARTESIAN_POINT('Ctrl Pts',(-50.2715679782614,17.5625898545436,3.95224981457436));
#19833=CARTESIAN_POINT('Ctrl Pts',(-49.3229272811221,17.6659872998999,10.4928580226408));
#19834=CARTESIAN_POINT('Ctrl Pts',(-44.9841390385641,17.874922814359,22.7664677855985));
#19835=CARTESIAN_POINT('Ctrl Pts',(-41.6627992432918,17.9739293100305,28.3918287722335));
#19836=CARTESIAN_POINT('Ctrl Pts',(-33.0577929465509,18.1820274332102,38.0674303707594));
#19837=CARTESIAN_POINT('Ctrl Pts',(-27.8540797746203,18.2836338165375,42.0249568859643));
#19838=CARTESIAN_POINT('Ctrl Pts',(-16.158841993745,18.489428753646,47.7685201871846));
#19839=CARTESIAN_POINT('Ctrl Pts',(-9.76613431960756,18.5959380618995,49.4728443301955));
#19840=CARTESIAN_POINT('Ctrl Pts',(-2.15216982670219,18.7163885934413,49.9652695656877));
#19841=CARTESIAN_POINT('Ctrl Pts',(-1.07595777047503,18.7332686288908,50.));
#19842=CARTESIAN_POINT('Ctrl Pts',(2.77555756156289E-16,18.75,50.));
#19843=CARTESIAN_POINT('Origin',(15.2417684546534,19.3910854416803,46.909359659535));
#19844=CARTESIAN_POINT('',(15.2417680422519,20.58,46.9093597935322));
#19845=CARTESIAN_POINT('',(15.4508438171073,19.0004604433873,47.5528277323164));
#19846=CARTESIAN_POINT('Origin',(-4.44089209850063E-14,2.18749999317203,
-8.4502213867173E-14));
#19847=CARTESIAN_POINT('Ctrl Pts',(-47.293670625,5.31249999317204,-4.77048955893622E-15));
#19848=CARTESIAN_POINT('Ctrl Pts',(-47.293670625,5.52083332650537,12.6723008510722));
#19849=CARTESIAN_POINT('Ctrl Pts',(-40.9575201994638,5.7291666598387,23.6468353125));
#19850=CARTESIAN_POINT('Ctrl Pts',(-34.6213697739277,5.93749999317203,34.6213697739277));
#19851=CARTESIAN_POINT('Ctrl Pts',(-23.6468353125,6.14583332650537,40.9575201994638));
#19852=CARTESIAN_POINT('Ctrl Pts',(-12.6723008510723,6.3541666598387,47.293670625));
#19853=CARTESIAN_POINT('Ctrl Pts',(-2.77555756156289E-14,6.56249999317203,
47.293670625));
#19854=CARTESIAN_POINT('Ctrl Pts',(12.6723008510722,6.77083332650537,47.293670625));
#19855=CARTESIAN_POINT('Ctrl Pts',(23.6468353125,6.9791666598387,40.9575201994639));
#19856=CARTESIAN_POINT('Ctrl Pts',(34.6213697739277,7.18749999317204,34.6213697739278));
#19857=CARTESIAN_POINT('Ctrl Pts',(40.9575201994639,7.39583332650537,23.6468353125));
#19858=CARTESIAN_POINT('Ctrl Pts',(47.293670625,7.6041666598387,12.6723008510723));
#19859=CARTESIAN_POINT('Ctrl Pts',(47.293670625,7.81249999317203,4.33680868994202E-16));
#19860=CARTESIAN_POINT('Ctrl Pts',(47.293670625,8.02083332650537,-12.6723008510723));
#19861=CARTESIAN_POINT('Ctrl Pts',(40.9575201994639,8.2291666598387,-23.6468353125));
#19862=CARTESIAN_POINT('Ctrl Pts',(34.6213697739278,8.43749999317204,-34.6213697739277));
#19863=CARTESIAN_POINT('Ctrl Pts',(23.6468353125,8.64583332650537,-40.9575201994639));
#19864=CARTESIAN_POINT('Ctrl Pts',(12.6723008510723,8.8541666598387,-47.293670625));
#19865=CARTESIAN_POINT('Ctrl Pts',(0.,9.06249999317203,-47.293670625));
#19866=CARTESIAN_POINT('Ctrl Pts',(-12.6723008510723,9.27083332650536,-47.293670625));
#19867=CARTESIAN_POINT('Ctrl Pts',(-23.6468353125,9.4791666598387,-40.9575201994639));
#19868=CARTESIAN_POINT('Ctrl Pts',(-34.6213697739277,9.68749999317203,-34.6213697739277));
#19869=CARTESIAN_POINT('Ctrl Pts',(-40.9575201994638,9.89583332650537,-23.6468353125));
#19870=CARTESIAN_POINT('Ctrl Pts',(-47.293670625,10.1041666598387,-12.6723008510723));
#19871=CARTESIAN_POINT('Ctrl Pts',(-47.293670625,10.312499993172,-4.77048955893622E-15));
#19872=CARTESIAN_POINT('Ctrl Pts',(-47.293670625,4.06249999317204,-5.20417042793042E-15));
#19873=CARTESIAN_POINT('Ctrl Pts',(-47.293670625,4.27083332650536,12.6723008510722));
#19874=CARTESIAN_POINT('Ctrl Pts',(-40.9575201994638,4.4791666598387,23.6468353125));
#19875=CARTESIAN_POINT('Ctrl Pts',(-34.6213697739277,4.68749999317204,34.6213697739277));
#19876=CARTESIAN_POINT('Ctrl Pts',(-23.6468353125,4.89583332650537,40.9575201994639));
#19877=CARTESIAN_POINT('Ctrl Pts',(-12.6723008510723,5.1041666598387,47.293670625));
#19878=CARTESIAN_POINT('Ctrl Pts',(-2.77555756156289E-14,5.31249999317204,
47.293670625));
#19879=CARTESIAN_POINT('Ctrl Pts',(12.6723008510722,5.52083332650537,47.293670625));
#19880=CARTESIAN_POINT('Ctrl Pts',(23.6468353125,5.7291666598387,40.9575201994639));
#19881=CARTESIAN_POINT('Ctrl Pts',(34.6213697739277,5.93749999317203,34.6213697739278));
#19882=CARTESIAN_POINT('Ctrl Pts',(40.9575201994639,6.14583332650537,23.6468353125));
#19883=CARTESIAN_POINT('Ctrl Pts',(47.293670625,6.3541666598387,12.6723008510723));
#19884=CARTESIAN_POINT('Ctrl Pts',(47.293670625,6.56249999317203,0.));
#19885=CARTESIAN_POINT('Ctrl Pts',(47.293670625,6.77083332650537,-12.6723008510723));
#19886=CARTESIAN_POINT('Ctrl Pts',(40.9575201994639,6.9791666598387,-23.6468353125));
#19887=CARTESIAN_POINT('Ctrl Pts',(34.6213697739278,7.18749999317204,-34.6213697739277));
#19888=CARTESIAN_POINT('Ctrl Pts',(23.6468353125,7.39583332650537,-40.9575201994639));
#19889=CARTESIAN_POINT('Ctrl Pts',(12.6723008510723,7.6041666598387,-47.293670625));
#19890=CARTESIAN_POINT('Ctrl Pts',(0.,7.81249999317203,-47.293670625));
#19891=CARTESIAN_POINT('Ctrl Pts',(-12.6723008510723,8.02083332650537,-47.293670625));
#19892=CARTESIAN_POINT('Ctrl Pts',(-23.6468353125,8.2291666598387,-40.9575201994639));
#19893=CARTESIAN_POINT('Ctrl Pts',(-34.6213697739277,8.43749999317203,-34.6213697739278));
#19894=CARTESIAN_POINT('Ctrl Pts',(-40.9575201994638,8.64583332650537,-23.6468353125));
#19895=CARTESIAN_POINT('Ctrl Pts',(-47.293670625,8.8541666598387,-12.6723008510723));
#19896=CARTESIAN_POINT('Ctrl Pts',(-47.293670625,9.06249999317203,-5.20417042793042E-15));
#19897=CARTESIAN_POINT('Ctrl Pts',(50.,4.37499998634407,4.33680868994202E-16));
#19898=CARTESIAN_POINT('Ctrl Pts',(50.0000000000001,4.5833333196774,-13.3974596215561));
#19899=CARTESIAN_POINT('Ctrl Pts',(43.301270189222,4.79166665301074,-25.));
#19900=CARTESIAN_POINT('Ctrl Pts',(36.6025403784439,4.99999998634406,-36.6025403784439));
#19901=CARTESIAN_POINT('Ctrl Pts',(25.0000000000001,5.2083333196774,-43.3012701892219));
#19902=CARTESIAN_POINT('Ctrl Pts',(13.3974596215562,5.41666665301073,-50.));
#19903=CARTESIAN_POINT('Ctrl Pts',(2.77555756156289E-14,5.62499998634407,
-50.));
#19904=CARTESIAN_POINT('Ctrl Pts',(-13.3974596215561,5.8333333196774,-50.));
#19905=CARTESIAN_POINT('Ctrl Pts',(-25.,6.04166665301074,-43.301270189222));
#19906=CARTESIAN_POINT('Ctrl Pts',(-36.6025403784439,6.24999998634407,-36.6025403784439));
#19907=CARTESIAN_POINT('Ctrl Pts',(-43.3012701892219,6.4583333196774,-25.));
#19908=CARTESIAN_POINT('Ctrl Pts',(-50.,6.66666665301073,-13.3974596215561));
#19909=CARTESIAN_POINT('Ctrl Pts',(-50.,6.87499998634407,-5.63785129692462E-15));
#19910=CARTESIAN_POINT('Ctrl Pts',(-50.,7.0833333196774,13.3974596215561));
#19911=CARTESIAN_POINT('Ctrl Pts',(-43.3012701892219,7.29166665301073,25.));
#19912=CARTESIAN_POINT('Ctrl Pts',(-36.6025403784438,7.49999998634406,36.6025403784438));
#19913=CARTESIAN_POINT('Ctrl Pts',(-25.,7.7083333196774,43.3012701892219));
#19914=CARTESIAN_POINT('Ctrl Pts',(-13.3974596215562,7.91666665301074,50.));
#19915=CARTESIAN_POINT('Ctrl Pts',(0.,8.12499998634407,50.));
#19916=CARTESIAN_POINT('Ctrl Pts',(13.3974596215562,8.3333333196774,50.));
#19917=CARTESIAN_POINT('Ctrl Pts',(25.,8.54166665301073,43.301270189222));
#19918=CARTESIAN_POINT('Ctrl Pts',(36.6025403784438,8.74999998634407,36.6025403784439));
#19919=CARTESIAN_POINT('Ctrl Pts',(43.301270189222,8.9583333196774,25.));
#19920=CARTESIAN_POINT('Ctrl Pts',(50.,9.16666665301073,13.3974596215562));
#19921=CARTESIAN_POINT('Ctrl Pts',(50.,9.37499998634407,4.33680868994202E-16));
#19922=CARTESIAN_POINT('Ctrl Pts',(50.0000000000001,9.5833333196774,-13.3974596215561));
#19923=CARTESIAN_POINT('Ctrl Pts',(43.301270189222,9.79166665301073,-25.));
#19924=CARTESIAN_POINT('Ctrl Pts',(36.6025403784439,9.99999998634406,-36.6025403784439));
#19925=CARTESIAN_POINT('Ctrl Pts',(25.0000000000001,10.2083333196774,-43.3012701892219));
#19926=CARTESIAN_POINT('Ctrl Pts',(13.3974596215562,10.4166666530107,-50.));
#19927=CARTESIAN_POINT('Ctrl Pts',(2.77555756156289E-14,10.6249999863441,
-50.));
#19928=CARTESIAN_POINT('Ctrl Pts',(-13.3974596215561,10.8333333196774,-50.));
#19929=CARTESIAN_POINT('Ctrl Pts',(-25.,11.0416666530107,-43.301270189222));
#19930=CARTESIAN_POINT('Ctrl Pts',(-36.6025403784439,11.2499999863441,-36.6025403784439));
#19931=CARTESIAN_POINT('Ctrl Pts',(-43.3012701892219,11.4583333196774,-25.));
#19932=CARTESIAN_POINT('Ctrl Pts',(-50.,11.6666666530107,-13.3974596215561));
#19933=CARTESIAN_POINT('Ctrl Pts',(-50.,11.8749999863441,-5.63785129692462E-15));
#19934=CARTESIAN_POINT('Ctrl Pts',(-50.,12.0833333196774,13.3974596215561));
#19935=CARTESIAN_POINT('Ctrl Pts',(-43.3012701892219,12.2916666530107,25.));
#19936=CARTESIAN_POINT('Ctrl Pts',(-36.6025403784438,12.4999999863441,36.6025403784438));
#19937=CARTESIAN_POINT('Ctrl Pts',(-25.,12.7083333196774,43.3012701892219));
#19938=CARTESIAN_POINT('Ctrl Pts',(-13.3974596215562,12.9166666530107,50.));
#19939=CARTESIAN_POINT('Ctrl Pts',(0.,13.1249999863441,50.));
#19940=CARTESIAN_POINT('Ctrl Pts',(13.3974596215562,13.3333333196774,50.));
#19941=CARTESIAN_POINT('Ctrl Pts',(25.,13.5416666530107,43.301270189222));
#19942=CARTESIAN_POINT('Ctrl Pts',(36.6025403784438,13.7499999863441,36.6025403784439));
#19943=CARTESIAN_POINT('Ctrl Pts',(43.301270189222,13.9583333196774,25.));
#19944=CARTESIAN_POINT('Ctrl Pts',(50.,14.1666666530107,13.3974596215562));
#19945=CARTESIAN_POINT('Ctrl Pts',(50.,14.3749999863441,4.33680868994202E-16));
#19946=CARTESIAN_POINT('Ctrl Pts',(50.0000000000001,14.5833333196774,-13.3974596215561));
#19947=CARTESIAN_POINT('Ctrl Pts',(43.301270189222,14.7916666530107,-25.));
#19948=CARTESIAN_POINT('Ctrl Pts',(36.6025403784439,14.9999999863441,-36.6025403784439));
#19949=CARTESIAN_POINT('Ctrl Pts',(25.0000000000001,15.2083333196774,-43.3012701892219));
#19950=CARTESIAN_POINT('Ctrl Pts',(13.3974596215562,15.4166666530107,-50.));
#19951=CARTESIAN_POINT('Ctrl Pts',(2.77555756156289E-14,15.6249999863441,
-50.));
#19952=CARTESIAN_POINT('Ctrl Pts',(-13.3974596215561,15.8333333196774,-50.));
#19953=CARTESIAN_POINT('Ctrl Pts',(-25.,16.0416666530107,-43.301270189222));
#19954=CARTESIAN_POINT('Ctrl Pts',(-36.6025403784439,16.2499999863441,-36.6025403784439));
#19955=CARTESIAN_POINT('Ctrl Pts',(-43.3012701892219,16.4583333196774,-25.));
#19956=CARTESIAN_POINT('Ctrl Pts',(-50.,16.6666666530107,-13.3974596215561));
#19957=CARTESIAN_POINT('Ctrl Pts',(-50.,16.8749999863441,-5.63785129692462E-15));
#19958=CARTESIAN_POINT('Ctrl Pts',(-50.,17.0833333196774,13.3974596215561));
#19959=CARTESIAN_POINT('Ctrl Pts',(-43.3012701892219,17.2916666530107,25.));
#19960=CARTESIAN_POINT('Ctrl Pts',(-36.6025403784438,17.4999999863441,36.6025403784438));
#19961=CARTESIAN_POINT('Ctrl Pts',(-25.,17.7083333196774,43.3012701892219));
#19962=CARTESIAN_POINT('Ctrl Pts',(-13.3974596215562,17.9166666530107,50.));
#19963=CARTESIAN_POINT('Ctrl Pts',(0.,18.1249999863441,50.));
#19964=CARTESIAN_POINT('Ctrl Pts',(13.3974596215562,18.3333333196774,50.));
#19965=CARTESIAN_POINT('Ctrl Pts',(25.,18.5416666530107,43.301270189222));
#19966=CARTESIAN_POINT('Ctrl Pts',(36.6025403784438,18.7499999863441,36.6025403784439));
#19967=CARTESIAN_POINT('Ctrl Pts',(43.301270189222,18.9583333196774,25.));
#19968=CARTESIAN_POINT('Ctrl Pts',(50.,19.1666666530107,13.3974596215562));
#19969=CARTESIAN_POINT('Ctrl Pts',(50.,19.3749999863441,4.33680868994202E-16));
#19970=CARTESIAN_POINT('Ctrl Pts',(50.0000000000001,19.5833333196774,-13.3974596215561));
#19971=CARTESIAN_POINT('Ctrl Pts',(43.301270189222,19.7916666530107,-25.));
#19972=CARTESIAN_POINT('Ctrl Pts',(36.6025403784439,19.9999999863441,-36.6025403784439));
#19973=CARTESIAN_POINT('Ctrl Pts',(25.0000000000001,20.2083333196774,-43.3012701892219));
#19974=CARTESIAN_POINT('Ctrl Pts',(13.3974596215562,20.4166666530107,-50.));
#19975=CARTESIAN_POINT('Ctrl Pts',(2.77555756156289E-14,20.6249999863441,
-50.));
#19976=CARTESIAN_POINT('Ctrl Pts',(-13.3974596215561,20.8333333196774,-50.));
#19977=CARTESIAN_POINT('Ctrl Pts',(-25.,21.0416666530107,-43.301270189222));
#19978=CARTESIAN_POINT('Ctrl Pts',(-36.6025403784439,21.2499999863441,-36.6025403784439));
#19979=CARTESIAN_POINT('Ctrl Pts',(-43.3012701892219,21.4583333196774,-25.));
#19980=CARTESIAN_POINT('Ctrl Pts',(-50.,21.6666666530107,-13.3974596215561));
#19981=CARTESIAN_POINT('Ctrl Pts',(-50.,21.8749999863441,-5.63785129692462E-15));
#19982=CARTESIAN_POINT('Ctrl Pts',(-50.,22.0833333196774,13.3974596215561));
#19983=CARTESIAN_POINT('Ctrl Pts',(-43.3012701892219,22.2916666530107,25.));
#19984=CARTESIAN_POINT('Ctrl Pts',(-36.6025403784438,22.4999999863441,36.6025403784438));
#19985=CARTESIAN_POINT('Ctrl Pts',(-25.,22.7083333196774,43.3012701892219));
#19986=CARTESIAN_POINT('Ctrl Pts',(-13.3974596215562,22.9166666530107,50.));
#19987=CARTESIAN_POINT('Ctrl Pts',(0.,23.1249999863441,50.));
#19988=CARTESIAN_POINT('Ctrl Pts',(7.91921917061262,23.2481455209316,50.));
#19989=CARTESIAN_POINT('Ctrl Pts',(15.4508444385251,23.3754604402358,47.5528275304056));
#19990=CARTESIAN_POINT('Ctrl Pts',(47.293670625,2.81249999317203,4.33680868994202E-16));
#19991=CARTESIAN_POINT('Ctrl Pts',(47.293670625,3.02083332650537,-12.6723008510723));
#19992=CARTESIAN_POINT('Ctrl Pts',(40.9575201994639,3.2291666598387,-23.6468353125));
#19993=CARTESIAN_POINT('Ctrl Pts',(34.6213697739278,3.43749999317203,-34.6213697739277));
#19994=CARTESIAN_POINT('Ctrl Pts',(23.6468353125,3.64583332650537,-40.9575201994639));
#19995=CARTESIAN_POINT('Ctrl Pts',(12.6723008510723,3.8541666598387,-47.293670625));
#19996=CARTESIAN_POINT('Ctrl Pts',(0.,4.06249999317204,-47.293670625));
#19997=CARTESIAN_POINT('Ctrl Pts',(-12.6723008510723,4.27083332650536,-47.293670625));
#19998=CARTESIAN_POINT('Ctrl Pts',(-23.6468353125,4.4791666598387,-40.9575201994639));
#19999=CARTESIAN_POINT('Ctrl Pts',(-34.6213697739277,4.68749999317204,-34.6213697739277));
#20000=CARTESIAN_POINT('Ctrl Pts',(-40.9575201994638,4.89583332650537,-23.6468353125));
#20001=CARTESIAN_POINT('Ctrl Pts',(-47.293670625,5.1041666598387,-12.6723008510723));
#20002=CARTESIAN_POINT('Ctrl Pts',(-47.293670625,5.31249999317204,-4.77048955893622E-15));
#20003=CARTESIAN_POINT('Ctrl Pts',(-47.293670625,5.52083332650537,12.6723008510722));
#20004=CARTESIAN_POINT('Ctrl Pts',(-40.9575201994638,5.7291666598387,23.6468353125));
#20005=CARTESIAN_POINT('Ctrl Pts',(-34.6213697739277,5.93749999317203,34.6213697739277));
#20006=CARTESIAN_POINT('Ctrl Pts',(-23.6468353125,6.14583332650537,40.9575201994638));
#20007=CARTESIAN_POINT('Ctrl Pts',(-12.6723008510723,6.3541666598387,47.293670625));
#20008=CARTESIAN_POINT('Ctrl Pts',(-2.77555756156289E-14,6.56249999317203,
47.293670625));
#20009=CARTESIAN_POINT('Ctrl Pts',(12.6723008510722,6.77083332650537,47.293670625));
#20010=CARTESIAN_POINT('Ctrl Pts',(23.6468353125,6.9791666598387,40.9575201994639));
#20011=CARTESIAN_POINT('Ctrl Pts',(34.6213697739277,7.18749999317204,34.6213697739278));
#20012=CARTESIAN_POINT('Ctrl Pts',(40.9575201994639,7.39583332650537,23.6468353125));
#20013=CARTESIAN_POINT('Ctrl Pts',(47.293670625,7.6041666598387,12.6723008510723));
#20014=CARTESIAN_POINT('Ctrl Pts',(47.293670625,7.81249999317203,4.33680868994202E-16));
#20015=CARTESIAN_POINT('Ctrl Pts',(47.293670625,8.02083332650537,-12.6723008510723));
#20016=CARTESIAN_POINT('Ctrl Pts',(40.9575201994639,8.2291666598387,-23.6468353125));
#20017=CARTESIAN_POINT('Ctrl Pts',(34.6213697739278,8.43749999317204,-34.6213697739277));
#20018=CARTESIAN_POINT('Ctrl Pts',(23.6468353125,8.64583332650537,-40.9575201994639));
#20019=CARTESIAN_POINT('Ctrl Pts',(12.6723008510723,8.8541666598387,-47.293670625));
#20020=CARTESIAN_POINT('Ctrl Pts',(0.,9.06249999317203,-47.293670625));
#20021=CARTESIAN_POINT('Ctrl Pts',(-12.6723008510723,9.27083332650537,-47.293670625));
#20022=CARTESIAN_POINT('Ctrl Pts',(-23.6468353125,9.4791666598387,-40.9575201994639));
#20023=CARTESIAN_POINT('Ctrl Pts',(-34.6213697739277,9.68749999317203,-34.6213697739277));
#20024=CARTESIAN_POINT('Ctrl Pts',(-40.9575201994638,9.89583332650537,-23.6468353125));
#20025=CARTESIAN_POINT('Ctrl Pts',(-47.293670625,10.1041666598387,-12.6723008510723));
#20026=CARTESIAN_POINT('Ctrl Pts',(-47.293670625,10.312499993172,-4.77048955893622E-15));
#20027=CARTESIAN_POINT('Ctrl Pts',(-47.293670625,10.5208333265054,12.6723008510722));
#20028=CARTESIAN_POINT('Ctrl Pts',(-40.9575201994638,10.7291666598387,23.6468353125));
#20029=CARTESIAN_POINT('Ctrl Pts',(-34.6213697739277,10.937499993172,34.6213697739277));
#20030=CARTESIAN_POINT('Ctrl Pts',(-23.6468353125,11.1458333265054,40.9575201994638));
#20031=CARTESIAN_POINT('Ctrl Pts',(-12.6723008510723,11.3541666598387,47.293670625));
#20032=CARTESIAN_POINT('Ctrl Pts',(-2.77555756156289E-14,11.562499993172,
47.293670625));
#20033=CARTESIAN_POINT('Ctrl Pts',(12.6723008510722,11.7708333265054,47.293670625));
#20034=CARTESIAN_POINT('Ctrl Pts',(23.6468353125,11.9791666598387,40.9575201994639));
#20035=CARTESIAN_POINT('Ctrl Pts',(34.6213697739277,12.187499993172,34.6213697739278));
#20036=CARTESIAN_POINT('Ctrl Pts',(40.9575201994639,12.3958333265054,23.6468353125));
#20037=CARTESIAN_POINT('Ctrl Pts',(47.293670625,12.6041666598387,12.6723008510723));
#20038=CARTESIAN_POINT('Ctrl Pts',(47.293670625,12.812499993172,4.33680868994202E-16));
#20039=CARTESIAN_POINT('Ctrl Pts',(47.293670625,13.0208333265054,-12.6723008510723));
#20040=CARTESIAN_POINT('Ctrl Pts',(40.9575201994639,13.2291666598387,-23.6468353125));
#20041=CARTESIAN_POINT('Ctrl Pts',(34.6213697739278,13.437499993172,-34.6213697739277));
#20042=CARTESIAN_POINT('Ctrl Pts',(23.6468353125,13.6458333265054,-40.9575201994639));
#20043=CARTESIAN_POINT('Ctrl Pts',(12.6723008510723,13.8541666598387,-47.293670625));
#20044=CARTESIAN_POINT('Ctrl Pts',(0.,14.062499993172,-47.293670625));
#20045=CARTESIAN_POINT('Ctrl Pts',(-12.6723008510723,14.2708333265054,-47.293670625));
#20046=CARTESIAN_POINT('Ctrl Pts',(-23.6468353125,14.4791666598387,-40.9575201994639));
#20047=CARTESIAN_POINT('Ctrl Pts',(-34.6213697739277,14.687499993172,-34.6213697739277));
#20048=CARTESIAN_POINT('Ctrl Pts',(-40.9575201994638,14.8958333265054,-23.6468353125));
#20049=CARTESIAN_POINT('Ctrl Pts',(-47.293670625,15.1041666598387,-12.6723008510723));
#20050=CARTESIAN_POINT('Ctrl Pts',(-47.293670625,15.312499993172,-4.77048955893622E-15));
#20051=CARTESIAN_POINT('Ctrl Pts',(-47.293670625,15.5208333265054,12.6723008510722));
#20052=CARTESIAN_POINT('Ctrl Pts',(-40.9575201994638,15.7291666598387,23.6468353125));
#20053=CARTESIAN_POINT('Ctrl Pts',(-34.6213697739277,15.937499993172,34.6213697739277));
#20054=CARTESIAN_POINT('Ctrl Pts',(-23.6468353125,16.1458333265054,40.9575201994638));
#20055=CARTESIAN_POINT('Ctrl Pts',(-12.6723008510723,16.3541666598387,47.293670625));
#20056=CARTESIAN_POINT('Ctrl Pts',(-2.77555756156289E-14,16.562499993172,
47.293670625));
#20057=CARTESIAN_POINT('Ctrl Pts',(12.6723008510722,16.7708333265054,47.293670625));
#20058=CARTESIAN_POINT('Ctrl Pts',(23.6468353125,16.9791666598387,40.9575201994639));
#20059=CARTESIAN_POINT('Ctrl Pts',(34.6213697739277,17.187499993172,34.6213697739278));
#20060=CARTESIAN_POINT('Ctrl Pts',(40.9575201994639,17.3958333265054,23.6468353125));
#20061=CARTESIAN_POINT('Ctrl Pts',(47.293670625,17.6041666598387,12.6723008510723));
#20062=CARTESIAN_POINT('Ctrl Pts',(47.293670625,17.812499993172,4.33680868994202E-16));
#20063=CARTESIAN_POINT('Ctrl Pts',(47.293670625,18.0208333265054,-12.6723008510723));
#20064=CARTESIAN_POINT('Ctrl Pts',(40.9575201994639,18.2291666598387,-23.6468353125));
#20065=CARTESIAN_POINT('Ctrl Pts',(34.6213697739278,18.437499993172,-34.6213697739277));
#20066=CARTESIAN_POINT('Ctrl Pts',(23.6468353125,18.6458333265054,-40.9575201994639));
#20067=CARTESIAN_POINT('Ctrl Pts',(12.6723008510723,18.8541666598387,-47.293670625));
#20068=CARTESIAN_POINT('Ctrl Pts',(0.,19.062499993172,-47.293670625));
#20069=CARTESIAN_POINT('Ctrl Pts',(-12.6723008510723,19.2708333265054,-47.293670625));
#20070=CARTESIAN_POINT('Ctrl Pts',(-23.6468353125,19.4791666598387,-40.9575201994639));
#20071=CARTESIAN_POINT('Ctrl Pts',(-34.6213697739277,19.687499993172,-34.6213697739277));
#20072=CARTESIAN_POINT('Ctrl Pts',(-40.9575201994638,19.8958333265054,-23.6468353125));
#20073=CARTESIAN_POINT('Ctrl Pts',(-47.293670625,20.1041666598387,-12.6723008510723));
#20074=CARTESIAN_POINT('Ctrl Pts',(-47.293670625,20.312499993172,-4.77048955893622E-15));
#20075=CARTESIAN_POINT('Ctrl Pts',(-47.293670625,20.5208333265054,12.6723008510722));
#20076=CARTESIAN_POINT('Ctrl Pts',(-40.9575201994638,20.7291666598387,23.6468353125));
#20077=CARTESIAN_POINT('Ctrl Pts',(-34.6213697739277,20.937499993172,34.6213697739277));
#20078=CARTESIAN_POINT('Ctrl Pts',(-23.6468353125,21.1458333265054,40.9575201994638));
#20079=CARTESIAN_POINT('Ctrl Pts',(-12.6723008510723,21.3541666598387,47.293670625));
#20080=CARTESIAN_POINT('Ctrl Pts',(-2.77555756156289E-14,21.562499993172,
47.293670625));
#20081=CARTESIAN_POINT('Ctrl Pts',(7.49057886124279,21.6856455277595,47.293670625));
#20082=CARTESIAN_POINT('Ctrl Pts',(14.6145429550743,21.8129604470638,44.9789552502087));
#20083=CARTESIAN_POINT('Ctrl Pts',(-44.6588684919844,20.58,15.5652416043447));
#20084=CARTESIAN_POINT('Ctrl Pts',(-45.8223695666528,20.58,12.5182222321844));
#20085=CARTESIAN_POINT('Ctrl Pts',(-46.6680986770167,20.58,9.35920006449212));
#20086=CARTESIAN_POINT('Ctrl Pts',(-47.7115459842877,20.58,2.82738845179393));
#20087=CARTESIAN_POINT('Ctrl Pts',(-47.8846290450767,20.58,-0.526241684364264));
#20088=CARTESIAN_POINT('Ctrl Pts',(-47.3912185290812,20.58,-9.99324512899516));
#20089=CARTESIAN_POINT('Ctrl Pts',(-45.8995255488925,20.58,-16.0093794384006));
#20090=CARTESIAN_POINT('Ctrl Pts',(-41.9677631661302,20.58,-24.4923235135627));
#20091=CARTESIAN_POINT('Ctrl Pts',(-40.327232006205,20.58,-27.2658254068393));
#20092=CARTESIAN_POINT('Ctrl Pts',(-36.5713996983444,20.58,-32.3974946095854));
#20093=CARTESIAN_POINT('Ctrl Pts',(-34.4608877029428,20.58,-34.761199114609));
#20094=CARTESIAN_POINT('Ctrl Pts',(-27.0961825388857,20.58,-41.551889627277));
#20095=CARTESIAN_POINT('Ctrl Pts',(-21.4281170361254,20.5799999999902,-44.8194014831955));
#20096=CARTESIAN_POINT('Ctrl Pts',(-12.7851969301205,20.5799999999902,-47.9873865019175));
#20097=CARTESIAN_POINT('Ctrl Pts',(-9.76123390768821,20.58,-48.7819503108552));
#20098=CARTESIAN_POINT('Ctrl Pts',(-3.52062841150329,20.58,-49.8054784288519));
#20099=CARTESIAN_POINT('Ctrl Pts',(-0.322512932949123,20.58,-50.0138607547272));
#20100=CARTESIAN_POINT('Ctrl Pts',(2.87173475049018,20.58,-49.9174632721138));
#20101=CARTESIAN_POINT('',(50.,4.37499998634407,4.33680868994202E-16));
#20102=CARTESIAN_POINT('Origin',(0.,30.,0.));
#20103=CARTESIAN_POINT('Origin',(0.,0.,0.));
#20104=CARTESIAN_POINT('Origin',(48.6468353125001,0.78124999658602,4.33680868994202E-16));
#20105=CARTESIAN_POINT('',(47.293670625,1.56249999317203,0.));
#20106=CARTESIAN_POINT('Ctrl Pts',(47.293670625,1.56249999317203,0.));
#20107=CARTESIAN_POINT('Ctrl Pts',(47.293670625,1.77083332650536,-12.6723008510723));
#20108=CARTESIAN_POINT('Ctrl Pts',(40.9575201994639,1.9791666598387,-23.6468353125));
#20109=CARTESIAN_POINT('Ctrl Pts',(34.6213697739278,2.18749999317203,-34.6213697739277));
#20110=CARTESIAN_POINT('Ctrl Pts',(23.6468353125,2.39583332650536,-40.9575201994639));
#20111=CARTESIAN_POINT('Ctrl Pts',(12.6723008510723,2.6041666598387,-47.293670625));
#20112=CARTESIAN_POINT('Ctrl Pts',(0.,2.81249999317203,-47.293670625));
#20113=CARTESIAN_POINT('Ctrl Pts',(-12.6723008510723,3.02083332650537,-47.293670625));
#20114=CARTESIAN_POINT('Ctrl Pts',(-23.6468353125,3.2291666598387,-40.9575201994639));
#20115=CARTESIAN_POINT('Ctrl Pts',(-34.6213697739277,3.43749999317203,-34.6213697739278));
#20116=CARTESIAN_POINT('Ctrl Pts',(-40.9575201994638,3.64583332650537,-23.6468353125));
#20117=CARTESIAN_POINT('Ctrl Pts',(-47.293670625,3.8541666598387,-12.6723008510723));
#20118=CARTESIAN_POINT('Ctrl Pts',(-47.293670625,4.06249999317204,-5.20417042793042E-15));
#20119=CARTESIAN_POINT('Ctrl Pts',(-47.293670625,4.27083332650536,12.6723008510722));
#20120=CARTESIAN_POINT('Ctrl Pts',(-40.9575201994638,4.4791666598387,23.6468353125));
#20121=CARTESIAN_POINT('Ctrl Pts',(-34.6213697739277,4.68749999317204,34.6213697739277));
#20122=CARTESIAN_POINT('Ctrl Pts',(-23.6468353125,4.89583332650537,40.9575201994639));
#20123=CARTESIAN_POINT('Ctrl Pts',(-12.6723008510723,5.1041666598387,47.293670625));
#20124=CARTESIAN_POINT('Ctrl Pts',(-2.77555756156289E-14,5.31249999317204,
47.293670625));
#20125=CARTESIAN_POINT('Ctrl Pts',(12.6723008510722,5.52083332650537,47.293670625));
#20126=CARTESIAN_POINT('Ctrl Pts',(23.6468353125,5.7291666598387,40.9575201994639));
#20127=CARTESIAN_POINT('Ctrl Pts',(34.6213697739277,5.93749999317203,34.6213697739278));
#20128=CARTESIAN_POINT('Ctrl Pts',(40.9575201994639,6.14583332650537,23.6468353125));
#20129=CARTESIAN_POINT('Ctrl Pts',(47.293670625,6.3541666598387,12.6723008510723));
#20130=CARTESIAN_POINT('Ctrl Pts',(47.293670625,6.56249999317203,0.));
#20131=CARTESIAN_POINT('Ctrl Pts',(47.293670625,6.77083332650537,-12.6723008510723));
#20132=CARTESIAN_POINT('Ctrl Pts',(40.9575201994639,6.9791666598387,-23.6468353125));
#20133=CARTESIAN_POINT('Ctrl Pts',(34.6213697739278,7.18749999317204,-34.6213697739277));
#20134=CARTESIAN_POINT('Ctrl Pts',(23.6468353125,7.39583332650537,-40.9575201994639));
#20135=CARTESIAN_POINT('Ctrl Pts',(12.6723008510723,7.6041666598387,-47.293670625));
#20136=CARTESIAN_POINT('Ctrl Pts',(0.,7.81249999317203,-47.293670625));
#20137=CARTESIAN_POINT('Ctrl Pts',(-12.6723008510723,8.02083332650537,-47.293670625));
#20138=CARTESIAN_POINT('Ctrl Pts',(-23.6468353125,8.2291666598387,-40.9575201994639));
#20139=CARTESIAN_POINT('Ctrl Pts',(-34.6213697739277,8.43749999317203,-34.6213697739278));
#20140=CARTESIAN_POINT('Ctrl Pts',(-40.9575201994638,8.64583332650537,-23.6468353125));
#20141=CARTESIAN_POINT('Ctrl Pts',(-47.293670625,8.8541666598387,-12.6723008510723));
#20142=CARTESIAN_POINT('Ctrl Pts',(-47.293670625,9.06249999317203,-5.20417042793042E-15));
#20143=CARTESIAN_POINT('Ctrl Pts',(-47.293670625,9.27083332650537,12.6723008510722));
#20144=CARTESIAN_POINT('Ctrl Pts',(-40.9575201994638,9.4791666598387,23.6468353125));
#20145=CARTESIAN_POINT('Ctrl Pts',(-34.6213697739277,9.68749999317203,34.6213697739277));
#20146=CARTESIAN_POINT('Ctrl Pts',(-23.6468353125,9.89583332650536,40.9575201994639));
#20147=CARTESIAN_POINT('Ctrl Pts',(-12.6723008510723,10.1041666598387,47.293670625));
#20148=CARTESIAN_POINT('Ctrl Pts',(-2.77555756156289E-14,10.312499993172,
47.293670625));
#20149=CARTESIAN_POINT('Ctrl Pts',(12.6723008510722,10.5208333265054,47.293670625));
#20150=CARTESIAN_POINT('Ctrl Pts',(23.6468353125,10.7291666598387,40.9575201994639));
#20151=CARTESIAN_POINT('Ctrl Pts',(34.6213697739277,10.937499993172,34.6213697739278));
#20152=CARTESIAN_POINT('Ctrl Pts',(40.9575201994639,11.1458333265054,23.6468353125));
#20153=CARTESIAN_POINT('Ctrl Pts',(47.293670625,11.3541666598387,12.6723008510723));
#20154=CARTESIAN_POINT('Ctrl Pts',(47.293670625,11.562499993172,0.));
#20155=CARTESIAN_POINT('Ctrl Pts',(47.293670625,11.7708333265054,-12.6723008510723));
#20156=CARTESIAN_POINT('Ctrl Pts',(40.9575201994639,11.9791666598387,-23.6468353125));
#20157=CARTESIAN_POINT('Ctrl Pts',(34.6213697739278,12.187499993172,-34.6213697739277));
#20158=CARTESIAN_POINT('Ctrl Pts',(23.6468353125,12.3958333265054,-40.9575201994639));
#20159=CARTESIAN_POINT('Ctrl Pts',(12.6723008510723,12.6041666598387,-47.293670625));
#20160=CARTESIAN_POINT('Ctrl Pts',(0.,12.812499993172,-47.293670625));
#20161=CARTESIAN_POINT('Ctrl Pts',(-12.6723008510723,13.0208333265054,-47.293670625));
#20162=CARTESIAN_POINT('Ctrl Pts',(-23.6468353125,13.2291666598387,-40.9575201994639));
#20163=CARTESIAN_POINT('Ctrl Pts',(-34.6213697739277,13.437499993172,-34.6213697739278));
#20164=CARTESIAN_POINT('Ctrl Pts',(-40.9575201994638,13.6458333265054,-23.6468353125));
#20165=CARTESIAN_POINT('Ctrl Pts',(-47.293670625,13.8541666598387,-12.6723008510723));
#20166=CARTESIAN_POINT('Ctrl Pts',(-47.293670625,14.062499993172,-5.20417042793042E-15));
#20167=CARTESIAN_POINT('Ctrl Pts',(-47.293670625,14.2708333265054,12.6723008510722));
#20168=CARTESIAN_POINT('Ctrl Pts',(-40.9575201994638,14.4791666598387,23.6468353125));
#20169=CARTESIAN_POINT('Ctrl Pts',(-34.6213697739277,14.687499993172,34.6213697739277));
#20170=CARTESIAN_POINT('Ctrl Pts',(-23.6468353125,14.8958333265054,40.9575201994639));
#20171=CARTESIAN_POINT('Ctrl Pts',(-12.6723008510723,15.1041666598387,47.293670625));
#20172=CARTESIAN_POINT('Ctrl Pts',(-2.77555756156289E-14,15.312499993172,
47.293670625));
#20173=CARTESIAN_POINT('Ctrl Pts',(12.6723008510722,15.5208333265054,47.293670625));
#20174=CARTESIAN_POINT('Ctrl Pts',(23.6468353125,15.7291666598387,40.9575201994639));
#20175=CARTESIAN_POINT('Ctrl Pts',(34.6213697739277,15.937499993172,34.6213697739278));
#20176=CARTESIAN_POINT('Ctrl Pts',(40.9575201994639,16.1458333265054,23.6468353125));
#20177=CARTESIAN_POINT('Ctrl Pts',(47.293670625,16.3541666598387,12.6723008510723));
#20178=CARTESIAN_POINT('Ctrl Pts',(47.293670625,16.562499993172,0.));
#20179=CARTESIAN_POINT('Ctrl Pts',(47.293670625,16.7708333265054,-12.6723008510723));
#20180=CARTESIAN_POINT('Ctrl Pts',(40.9575201994639,16.9791666598387,-23.6468353125));
#20181=CARTESIAN_POINT('Ctrl Pts',(34.6213697739278,17.187499993172,-34.6213697739277));
#20182=CARTESIAN_POINT('Ctrl Pts',(23.6468353125,17.3958333265054,-40.9575201994639));
#20183=CARTESIAN_POINT('Ctrl Pts',(12.6723008510723,17.6041666598387,-47.293670625));
#20184=CARTESIAN_POINT('Ctrl Pts',(0.,17.812499993172,-47.293670625));
#20185=CARTESIAN_POINT('Ctrl Pts',(-12.6723008510723,18.0208333265054,-47.293670625));
#20186=CARTESIAN_POINT('Ctrl Pts',(-23.6468353125,18.2291666598387,-40.9575201994639));
#20187=CARTESIAN_POINT('Ctrl Pts',(-34.6213697739277,18.437499993172,-34.6213697739278));
#20188=CARTESIAN_POINT('Ctrl Pts',(-40.9575201994638,18.6458333265054,-23.6468353125));
#20189=CARTESIAN_POINT('Ctrl Pts',(-47.293670625,18.8541666598387,-12.6723008510723));
#20190=CARTESIAN_POINT('Ctrl Pts',(-47.293670625,19.062499993172,-5.20417042793042E-15));
#20191=CARTESIAN_POINT('Ctrl Pts',(-47.293670625,19.2708333265054,12.6723008510722));
#20192=CARTESIAN_POINT('Ctrl Pts',(-40.9575201994638,19.4791666598387,23.6468353125));
#20193=CARTESIAN_POINT('Ctrl Pts',(-34.6213697739277,19.687499993172,34.6213697739277));
#20194=CARTESIAN_POINT('Ctrl Pts',(-23.6468353125,19.8958333265054,40.9575201994639));
#20195=CARTESIAN_POINT('Ctrl Pts',(-12.6723008510723,20.1041666598387,47.293670625));
#20196=CARTESIAN_POINT('Ctrl Pts',(-2.77555756156289E-14,20.312499993172,
47.293670625));
#20197=CARTESIAN_POINT('Ctrl Pts',(7.49057854447537,20.4356455225519,47.293670625));
#20198=CARTESIAN_POINT('Ctrl Pts',(14.6145423672918,20.5629604365593,44.9789554411907));
#20199=CARTESIAN_POINT('Ctrl Pts',(20.0112685210152,20.65940726634,43.2254535591521));
#20200=CARTESIAN_POINT('Ctrl Pts',(25.4079946747386,20.7558540961206,41.4719516771133));
#20201=CARTESIAN_POINT('Ctrl Pts',(50.,0.,4.33680868994202E-16));
#20202=CARTESIAN_POINT('Ctrl Pts',(50.0000000000001,0.208333333333332,-13.3974596215561));
#20203=CARTESIAN_POINT('Ctrl Pts',(43.301270189222,0.416666666666669,-25.));
#20204=CARTESIAN_POINT('Ctrl Pts',(36.6025403784439,0.625000000000002,-36.6025403784439));
#20205=CARTESIAN_POINT('Ctrl Pts',(25.0000000000001,0.833333333333332,-43.3012701892219));
#20206=CARTESIAN_POINT('Ctrl Pts',(13.3974596215562,1.04166666666667,-50.));
#20207=CARTESIAN_POINT('Ctrl Pts',(2.77555756156289E-14,1.25,-50.));
#20208=CARTESIAN_POINT('Ctrl Pts',(-13.3974596215561,1.45833333333334,-50.));
#20209=CARTESIAN_POINT('Ctrl Pts',(-25.,1.66666666666666,-43.301270189222));
#20210=CARTESIAN_POINT('Ctrl Pts',(-36.6025403784439,1.875,-36.6025403784439));
#20211=CARTESIAN_POINT('Ctrl Pts',(-43.3012701892219,2.08333333333333,-25.));
#20212=CARTESIAN_POINT('Ctrl Pts',(-50.,2.29166666666667,-13.3974596215561));
#20213=CARTESIAN_POINT('Ctrl Pts',(-50.,2.5,-5.63785129692462E-15));
#20214=CARTESIAN_POINT('Ctrl Pts',(-50.,2.70833333333333,13.3974596215561));
#20215=CARTESIAN_POINT('Ctrl Pts',(-43.3012701892219,2.91666666666666,25.));
#20216=CARTESIAN_POINT('Ctrl Pts',(-36.6025403784438,3.125,36.6025403784438));
#20217=CARTESIAN_POINT('Ctrl Pts',(-25.,3.33333333333333,43.3012701892219));
#20218=CARTESIAN_POINT('Ctrl Pts',(-13.3974596215562,3.54166666666667,50.));
#20219=CARTESIAN_POINT('Ctrl Pts',(0.,3.75,50.));
#20220=CARTESIAN_POINT('Ctrl Pts',(13.3974596215562,3.95833333333334,50.));
#20221=CARTESIAN_POINT('Ctrl Pts',(25.,4.16666666666667,43.301270189222));
#20222=CARTESIAN_POINT('Ctrl Pts',(36.6025403784438,4.375,36.6025403784439));
#20223=CARTESIAN_POINT('Ctrl Pts',(43.301270189222,4.58333333333333,25.));
#20224=CARTESIAN_POINT('Ctrl Pts',(50.,4.79166666666667,13.3974596215562));
#20225=CARTESIAN_POINT('Ctrl Pts',(50.,5.,4.33680868994202E-16));
#20226=CARTESIAN_POINT('Ctrl Pts',(50.0000000000001,5.20833333333333,-13.3974596215561));
#20227=CARTESIAN_POINT('Ctrl Pts',(43.301270189222,5.41666666666667,-25.));
#20228=CARTESIAN_POINT('Ctrl Pts',(36.6025403784439,5.62499999999999,-36.6025403784439));
#20229=CARTESIAN_POINT('Ctrl Pts',(25.0000000000001,5.83333333333333,-43.3012701892219));
#20230=CARTESIAN_POINT('Ctrl Pts',(13.3974596215562,6.04166666666667,-50.));
#20231=CARTESIAN_POINT('Ctrl Pts',(2.77555756156289E-14,6.25,-50.));
#20232=CARTESIAN_POINT('Ctrl Pts',(-13.3974596215561,6.45833333333334,-50.));
#20233=CARTESIAN_POINT('Ctrl Pts',(-25.,6.66666666666667,-43.301270189222));
#20234=CARTESIAN_POINT('Ctrl Pts',(-36.6025403784439,6.875,-36.6025403784439));
#20235=CARTESIAN_POINT('Ctrl Pts',(-43.3012701892219,7.08333333333333,-25.));
#20236=CARTESIAN_POINT('Ctrl Pts',(-50.,7.29166666666666,-13.3974596215561));
#20237=CARTESIAN_POINT('Ctrl Pts',(-50.,7.5,-5.63785129692462E-15));
#20238=CARTESIAN_POINT('Ctrl Pts',(-50.,7.70833333333333,13.3974596215561));
#20239=CARTESIAN_POINT('Ctrl Pts',(-43.3012701892219,7.91666666666667,25.));
#20240=CARTESIAN_POINT('Ctrl Pts',(-36.6025403784438,8.125,36.6025403784438));
#20241=CARTESIAN_POINT('Ctrl Pts',(-25.,8.33333333333333,43.3012701892219));
#20242=CARTESIAN_POINT('Ctrl Pts',(-13.3974596215562,8.54166666666667,50.));
#20243=CARTESIAN_POINT('Ctrl Pts',(0.,8.75,50.));
#20244=CARTESIAN_POINT('Ctrl Pts',(13.3974596215562,8.95833333333333,50.));
#20245=CARTESIAN_POINT('Ctrl Pts',(25.,9.16666666666667,43.301270189222));
#20246=CARTESIAN_POINT('Ctrl Pts',(36.6025403784438,9.375,36.6025403784439));
#20247=CARTESIAN_POINT('Ctrl Pts',(43.301270189222,9.58333333333333,25.));
#20248=CARTESIAN_POINT('Ctrl Pts',(50.,9.79166666666667,13.3974596215562));
#20249=CARTESIAN_POINT('Ctrl Pts',(50.,10.,4.33680868994202E-16));
#20250=CARTESIAN_POINT('Ctrl Pts',(50.0000000000001,10.2083333333333,-13.3974596215561));
#20251=CARTESIAN_POINT('Ctrl Pts',(43.301270189222,10.4166666666667,-25.));
#20252=CARTESIAN_POINT('Ctrl Pts',(36.6025403784439,10.625,-36.6025403784439));
#20253=CARTESIAN_POINT('Ctrl Pts',(25.0000000000001,10.8333333333333,-43.3012701892219));
#20254=CARTESIAN_POINT('Ctrl Pts',(13.3974596215562,11.0416666666667,-50.));
#20255=CARTESIAN_POINT('Ctrl Pts',(2.77555756156289E-14,11.25,-50.));
#20256=CARTESIAN_POINT('Ctrl Pts',(-13.3974596215561,11.4583333333333,-50.));
#20257=CARTESIAN_POINT('Ctrl Pts',(-25.,11.6666666666667,-43.301270189222));
#20258=CARTESIAN_POINT('Ctrl Pts',(-36.6025403784439,11.875,-36.6025403784439));
#20259=CARTESIAN_POINT('Ctrl Pts',(-43.3012701892219,12.0833333333333,-25.));
#20260=CARTESIAN_POINT('Ctrl Pts',(-50.,12.2916666666667,-13.3974596215561));
#20261=CARTESIAN_POINT('Ctrl Pts',(-50.,12.5,-5.63785129692462E-15));
#20262=CARTESIAN_POINT('Ctrl Pts',(-50.,12.7083333333333,13.3974596215561));
#20263=CARTESIAN_POINT('Ctrl Pts',(-43.3012701892219,12.9166666666667,25.));
#20264=CARTESIAN_POINT('Ctrl Pts',(-36.6025403784438,13.125,36.6025403784438));
#20265=CARTESIAN_POINT('Ctrl Pts',(-25.,13.3333333333333,43.3012701892219));
#20266=CARTESIAN_POINT('Ctrl Pts',(-13.3974596215562,13.5416666666667,50.));
#20267=CARTESIAN_POINT('Ctrl Pts',(0.,13.75,50.));
#20268=CARTESIAN_POINT('Ctrl Pts',(13.3974596215562,13.9583333333333,50.));
#20269=CARTESIAN_POINT('Ctrl Pts',(25.,14.1666666666667,43.301270189222));
#20270=CARTESIAN_POINT('Ctrl Pts',(36.6025403784438,14.375,36.6025403784439));
#20271=CARTESIAN_POINT('Ctrl Pts',(43.301270189222,14.5833333333333,25.));
#20272=CARTESIAN_POINT('Ctrl Pts',(50.,14.7916666666667,13.3974596215562));
#20273=CARTESIAN_POINT('Ctrl Pts',(50.,15.,4.33680868994202E-16));
#20274=CARTESIAN_POINT('Ctrl Pts',(50.0000000000001,15.2083333333333,-13.3974596215561));
#20275=CARTESIAN_POINT('Ctrl Pts',(43.301270189222,15.4166666666667,-25.));
#20276=CARTESIAN_POINT('Ctrl Pts',(36.6025403784439,15.625,-36.6025403784439));
#20277=CARTESIAN_POINT('Ctrl Pts',(25.0000000000001,15.8333333333333,-43.3012701892219));
#20278=CARTESIAN_POINT('Ctrl Pts',(13.3974596215562,16.0416666666667,-50.));
#20279=CARTESIAN_POINT('Ctrl Pts',(2.77555756156289E-14,16.25,-50.));
#20280=CARTESIAN_POINT('Ctrl Pts',(-13.3974596215561,16.4583333333333,-50.));
#20281=CARTESIAN_POINT('Ctrl Pts',(-25.,16.6666666666667,-43.301270189222));
#20282=CARTESIAN_POINT('Ctrl Pts',(-36.6025403784439,16.875,-36.6025403784439));
#20283=CARTESIAN_POINT('Ctrl Pts',(-43.3012701892219,17.0833333333333,-25.));
#20284=CARTESIAN_POINT('Ctrl Pts',(-50.,17.2916666666667,-13.3974596215561));
#20285=CARTESIAN_POINT('Ctrl Pts',(-50.,17.5,-5.63785129692462E-15));
#20286=CARTESIAN_POINT('Ctrl Pts',(-50.,17.7083333333333,13.3974596215561));
#20287=CARTESIAN_POINT('Ctrl Pts',(-43.3012701892219,17.9166666666667,25.));
#20288=CARTESIAN_POINT('Ctrl Pts',(-36.6025403784438,18.125,36.6025403784438));
#20289=CARTESIAN_POINT('Ctrl Pts',(-25.,18.3333333333333,43.3012701892219));
#20290=CARTESIAN_POINT('Ctrl Pts',(-13.3974596215562,18.5416666666667,50.));
#20291=CARTESIAN_POINT('Ctrl Pts',(0.,18.75,50.));
#20292=CARTESIAN_POINT('Ctrl Pts',(7.91921883571848,18.8731455293798,50.));
#20293=CARTESIAN_POINT('Ctrl Pts',(15.4508438171073,19.0004604433872,47.5528277323164));
#20294=CARTESIAN_POINT('Ctrl Pts',(21.1563918137039,19.0969072731679,45.6989835932745));
#20295=CARTESIAN_POINT('Ctrl Pts',(26.8619398103006,19.1933541029486,43.8451394542326));
#20296=CARTESIAN_POINT('Origin',(0.,26.58,0.));
#20297=CARTESIAN_POINT('Origin',(0.,20.58,0.));
#20298=CARTESIAN_POINT('Origin',(0.,23.58,0.));
#20299=CARTESIAN_POINT('',(0.,0.,0.));
#20300=CARTESIAN_POINT('Origin',(0.,0.,3.42));
#20301=CARTESIAN_POINT('',(52.5,-3.51506025588257E-15,5.55111512312578E-16));
#20302=CARTESIAN_POINT('Origin',(0.,0.,0.));
#20303=CARTESIAN_POINT('',(52.5,-3.51506025588257E-15,3.42));
#20304=CARTESIAN_POINT('',(52.5,-3.51506025588257E-15,3.42));
#20305=CARTESIAN_POINT('Origin',(0.,0.,3.42));
#20306=CARTESIAN_POINT('Origin',(0.,0.,3.42));
#20307=CARTESIAN_POINT('Origin',(0.,0.,0.));
#20308=CARTESIAN_POINT('',(0.,0.,0.));
#20309=CARTESIAN_POINT('Origin',(0.,0.,3.42));
#20310=CARTESIAN_POINT('',(16.7,-2.04516015457608E-15,3.42));
#20311=CARTESIAN_POINT('Origin',(0.,0.,3.42));
#20312=CARTESIAN_POINT('',(16.7,-2.04516015457608E-15,0.));
#20313=CARTESIAN_POINT('',(16.7,-2.04516015457608E-15,3.42));
#20314=CARTESIAN_POINT('Origin',(0.,0.,0.));
#20315=CARTESIAN_POINT('Origin',(0.,0.,3.42));
#20316=CARTESIAN_POINT('',(40.,-4.89858719658941E-15,0.));
#20317=CARTESIAN_POINT('Origin',(0.,0.,0.));
#20318=CARTESIAN_POINT('',(40.,-4.89858719658941E-15,3.42));
#20319=CARTESIAN_POINT('',(40.,-4.89858719658941E-15,3.42));
#20320=CARTESIAN_POINT('Origin',(0.,0.,3.42));
#20321=CARTESIAN_POINT('Origin',(0.,0.,3.42));
#20322=CARTESIAN_POINT('Origin',(0.,0.,0.));
#20323=CARTESIAN_POINT('',(0.,0.,0.));
#20324=CARTESIAN_POINT('Origin',(0.,300.,0.));
#20325=CARTESIAN_POINT('',(-1.81247726273808E-15,300.,14.8));
#20326=CARTESIAN_POINT('Origin',(0.,300.,0.));
#20327=CARTESIAN_POINT('',(-1.81247726273808E-15,0.,14.8));
#20328=CARTESIAN_POINT('',(-1.81247726273808E-15,300.,14.8));
#20329=CARTESIAN_POINT('Origin',(0.,0.,0.));
#20330=CARTESIAN_POINT('Origin',(0.,300.,0.));
#20331=CARTESIAN_POINT('',(-2.04516015457608E-15,0.,16.7));
#20332=CARTESIAN_POINT('Origin',(0.,0.,0.));
#20333=CARTESIAN_POINT('',(-2.04516015457608E-15,300.,16.7));
#20334=CARTESIAN_POINT('',(-2.04516015457608E-15,300.,16.7));
#20335=CARTESIAN_POINT('Origin',(0.,300.,0.));
#20336=CARTESIAN_POINT('Origin',(0.,300.,0.));
#20337=CARTESIAN_POINT('Origin',(0.,0.,0.));
#20338=CARTESIAN_POINT('',(0.,0.,0.));
#20339=CARTESIAN_POINT('Origin',(0.,-13.475,0.));
#20340=CARTESIAN_POINT('',(-1.65327317884893E-15,0.,-13.5));
#20341=CARTESIAN_POINT('Origin',(0.,0.,0.));
#20342=CARTESIAN_POINT('',(-1.65327317884893E-15,6.525,-13.5));
#20343=CARTESIAN_POINT('',(-1.65327317884893E-15,-13.475,-13.5));
#20344=CARTESIAN_POINT('Origin',(0.,6.525,0.));
#20345=CARTESIAN_POINT('Origin',(0.,6.525,0.));
#20346=CARTESIAN_POINT('',(-2.04516015457608E-15,6.525,-16.7));
#20347=CARTESIAN_POINT('Origin',(0.,6.525,0.));
#20348=CARTESIAN_POINT('',(-2.04516015457608E-15,9.525,-16.7));
#20349=CARTESIAN_POINT('',(-2.04516015457608E-15,6.525,-16.7));
#20350=CARTESIAN_POINT('Origin',(0.,9.525,0.));
#20351=CARTESIAN_POINT('Origin',(-40.9338792388751,9.525,1.85445089342754E-12));
#20352=CARTESIAN_POINT('',(-40.9338792388751,9.525,5.00000000000185));
#20353=CARTESIAN_POINT('Origin',(-40.9338792388751,9.525,1.85445089342754E-12));
#20354=CARTESIAN_POINT('',(-40.9338792388751,0.,5.00000000000185));
#20355=CARTESIAN_POINT('',(-40.9338792388751,9.525,5.00000000000185));
#20356=CARTESIAN_POINT('Origin',(-40.9338792388751,0.,1.85445089342754E-12));
#20357=CARTESIAN_POINT('Origin',(3.69887587801777E-12,9.525,40.9338792388769));
#20358=CARTESIAN_POINT('',(3.6982635546182E-12,9.525,45.9338792388769));
#20359=CARTESIAN_POINT('Origin',(3.69887587801777E-12,9.525,40.9338792388769));
#20360=CARTESIAN_POINT('',(3.6982635546182E-12,0.,45.9338792388769));
#20361=CARTESIAN_POINT('',(3.6982635546182E-12,9.525,45.9338792388769));
#20362=CARTESIAN_POINT('Origin',(3.69887587801777E-12,0.,40.9338792388769));
#20363=CARTESIAN_POINT('Origin',(40.9338792388788,9.525,-1.84943793900889E-12));
#20364=CARTESIAN_POINT('',(40.9338792388788,9.525,4.99999999999815));
#20365=CARTESIAN_POINT('Origin',(40.9338792388788,9.525,-1.84943793900889E-12));
#20366=CARTESIAN_POINT('',(40.9338792388788,0.,4.99999999999815));
#20367=CARTESIAN_POINT('',(40.9338792388788,9.525,4.99999999999815));
#20368=CARTESIAN_POINT('Origin',(40.9338792388788,0.,-1.84943793900889E-12));
#20369=CARTESIAN_POINT('Origin',(0.,9.525,-40.9338792388769));
#20370=CARTESIAN_POINT('',(-6.12323399573676E-16,9.525,-35.9338792388769));
#20371=CARTESIAN_POINT('Origin',(0.,9.525,-40.9338792388769));
#20372=CARTESIAN_POINT('',(-6.12323399573676E-16,0.,-35.9338792388769));
#20373=CARTESIAN_POINT('',(-6.12323399573676E-16,9.525,-35.9338792388769));
#20374=CARTESIAN_POINT('Origin',(0.,0.,-40.9338792388769));
#20375=CARTESIAN_POINT('Origin',(0.,9.525,0.));
#20376=CARTESIAN_POINT('',(-6.12323399573677E-15,0.,50.));
#20377=CARTESIAN_POINT('Origin',(0.,0.,0.));
#20378=CARTESIAN_POINT('',(-6.12323399573677E-15,9.525,50.));
#20379=CARTESIAN_POINT('',(-6.12323399573677E-15,9.525,50.));
#20380=CARTESIAN_POINT('Origin',(0.,9.525,0.));
#20381=CARTESIAN_POINT('Origin',(0.,9.525,0.));
#20382=CARTESIAN_POINT('Origin',(0.,0.,0.));
#20383=CARTESIAN_POINT('Origin',(0.,6.525,0.));
#20384=CARTESIAN_POINT('',(0.,0.,0.));
#20385=CARTESIAN_POINT('Origin',(30.,9.53,4.7625));
#20386=CARTESIAN_POINT('',(30.,8.53,3.7625));
#20387=CARTESIAN_POINT('',(30.,1.,3.7625));
#20388=CARTESIAN_POINT('',(30.,9.53,3.7625));
#20389=CARTESIAN_POINT('',(30.,1.,-3.7625));
#20390=CARTESIAN_POINT('',(30.,1.,-4.7625));
#20391=CARTESIAN_POINT('',(30.,8.53,-3.7625));
#20392=CARTESIAN_POINT('',(30.,9.53,-3.7625));
#20393=CARTESIAN_POINT('',(30.,8.53,4.7625));
#20394=CARTESIAN_POINT('Origin',(-30.,9.53,-4.7625));
#20395=CARTESIAN_POINT('',(29.,8.53,-4.7625));
#20396=CARTESIAN_POINT('',(29.,1.,-4.7625));
#20397=CARTESIAN_POINT('',(29.,9.53,-4.7625));
#20398=CARTESIAN_POINT('',(-29.,1.,-4.7625));
#20399=CARTESIAN_POINT('',(-30.,1.,-4.7625));
#20400=CARTESIAN_POINT('',(-29.,8.53,-4.7625));
#20401=CARTESIAN_POINT('',(-29.,9.53,-4.7625));
#20402=CARTESIAN_POINT('',(-30.,8.53,-4.7625));
#20403=CARTESIAN_POINT('Origin',(-30.,9.53,4.7625));
#20404=CARTESIAN_POINT('',(-30.,8.53,-3.7625));
#20405=CARTESIAN_POINT('',(-30.,1.,-3.7625));
#20406=CARTESIAN_POINT('',(-30.,9.53,-3.7625));
#20407=CARTESIAN_POINT('',(-30.,1.,3.7625));
#20408=CARTESIAN_POINT('',(-30.,1.,4.7625));
#20409=CARTESIAN_POINT('',(-30.,8.53,3.7625));
#20410=CARTESIAN_POINT('',(-30.,9.53,3.7625));
#20411=CARTESIAN_POINT('',(-30.,8.53,4.7625));
#20412=CARTESIAN_POINT('Origin',(-30.,9.53,4.7625));
#20413=CARTESIAN_POINT('',(-29.,8.53,4.7625));
#20414=CARTESIAN_POINT('',(-29.,1.,4.7625));
#20415=CARTESIAN_POINT('',(-29.,9.53,4.7625));
#20416=CARTESIAN_POINT('',(29.,1.,4.7625));
#20417=CARTESIAN_POINT('',(30.,1.,4.7625));
#20418=CARTESIAN_POINT('',(29.,8.53,4.7625));
#20419=CARTESIAN_POINT('',(29.,9.53,4.7625));
#20420=CARTESIAN_POINT('',(-30.,8.53,4.7625));
#20421=CARTESIAN_POINT('Origin',(0.,9.53,0.));
#20422=CARTESIAN_POINT('',(-29.,9.53,-3.7625));
#20423=CARTESIAN_POINT('',(-29.,9.53,3.7625));
#20424=CARTESIAN_POINT('',(-29.,9.53,0.));
#20425=CARTESIAN_POINT('',(29.,9.53,3.7625));
#20426=CARTESIAN_POINT('',(0.,9.53,3.7625));
#20427=CARTESIAN_POINT('',(29.,9.53,-3.7625));
#20428=CARTESIAN_POINT('',(29.,9.53,0.));
#20429=CARTESIAN_POINT('',(0.,9.53,-3.7625));
#20430=CARTESIAN_POINT('Origin',(0.,0.,0.));
#20431=CARTESIAN_POINT('',(-29.,0.,3.7625));
#20432=CARTESIAN_POINT('',(-29.,0.,-3.7625));
#20433=CARTESIAN_POINT('',(-29.,0.,-4.7625));
#20434=CARTESIAN_POINT('',(29.,0.,-3.7625));
#20435=CARTESIAN_POINT('',(30.,0.,-3.7625));
#20436=CARTESIAN_POINT('',(29.,0.,3.7625));
#20437=CARTESIAN_POINT('',(29.,0.,4.7625));
#20438=CARTESIAN_POINT('',(-30.,0.,3.7625));
#20439=CARTESIAN_POINT('Origin',(-29.,9.53,-3.7625));
#20440=CARTESIAN_POINT('Origin',(-29.,8.53,-3.7625));
#20441=CARTESIAN_POINT('Origin',(-29.,1.,-3.7625));
#20442=CARTESIAN_POINT('Origin',(-29.,8.53,-3.7625));
#20443=CARTESIAN_POINT('Origin',(-29.,8.53,-3.7625));
#20444=CARTESIAN_POINT('Origin',(-29.,8.53,-3.7625));
#20445=CARTESIAN_POINT('Origin',(-29.,1.,-3.7625));
#20446=CARTESIAN_POINT('Origin',(-29.,1.,-3.7625));
#20447=CARTESIAN_POINT('Origin',(-29.,1.,-3.7625));
#20448=CARTESIAN_POINT('Origin',(-29.,8.53,0.));
#20449=CARTESIAN_POINT('Origin',(-29.,8.53,3.7625));
#20450=CARTESIAN_POINT('Origin',(0.,8.53,-3.7625));
#20451=CARTESIAN_POINT('Origin',(29.,8.53,-3.7625));
#20452=CARTESIAN_POINT('Origin',(29.,9.53,-3.7625));
#20453=CARTESIAN_POINT('Origin',(29.,1.,-3.7625));
#20454=CARTESIAN_POINT('Origin',(29.,8.53,-3.7625));
#20455=CARTESIAN_POINT('Origin',(-30.,1.,-3.7625));
#20456=CARTESIAN_POINT('Origin',(29.,1.,-3.7625));
#20457=CARTESIAN_POINT('Origin',(-29.,1.,4.7625));
#20458=CARTESIAN_POINT('Origin',(-29.,1.,3.7625));
#20459=CARTESIAN_POINT('Origin',(-29.,9.53,3.7625));
#20460=CARTESIAN_POINT('Origin',(-29.,8.53,3.7625));
#20461=CARTESIAN_POINT('Origin',(-29.,1.,3.7625));
#20462=CARTESIAN_POINT('Origin',(-29.,8.53,3.7625));
#20463=CARTESIAN_POINT('Origin',(-29.,8.53,3.7625));
#20464=CARTESIAN_POINT('Origin',(29.,8.53,-3.7625));
#20465=CARTESIAN_POINT('Origin',(29.,8.53,-3.7625));
#20466=CARTESIAN_POINT('Origin',(29.,1.,-3.7625));
#20467=CARTESIAN_POINT('Origin',(29.,1.,-3.7625));
#20468=CARTESIAN_POINT('Origin',(-29.,1.,3.7625));
#20469=CARTESIAN_POINT('Origin',(-29.,1.,3.7625));
#20470=CARTESIAN_POINT('Origin',(0.,8.53,3.7625));
#20471=CARTESIAN_POINT('Origin',(29.,8.53,3.7625));
#20472=CARTESIAN_POINT('Origin',(29.,8.53,0.));
#20473=CARTESIAN_POINT('Origin',(29.,8.53,3.7625));
#20474=CARTESIAN_POINT('Origin',(29.,1.,4.7625));
#20475=CARTESIAN_POINT('Origin',(29.,1.,3.7625));
#20476=CARTESIAN_POINT('Origin',(-30.,1.,3.7625));
#20477=CARTESIAN_POINT('Origin',(29.,1.,3.7625));
#20478=CARTESIAN_POINT('Origin',(29.,8.53,3.7625));
#20479=CARTESIAN_POINT('Origin',(29.,8.53,3.7625));
#20480=CARTESIAN_POINT('Origin',(29.,1.,3.7625));
#20481=CARTESIAN_POINT('Origin',(29.,1.,3.7625));
#20482=CARTESIAN_POINT('Origin',(29.,9.53,3.7625));
#20483=CARTESIAN_POINT('',(0.,0.,0.));
#20484=CARTESIAN_POINT('Origin',(6.93889390390723E-15,140.,0.));
#20485=CARTESIAN_POINT('',(2.19959845502478E-14,1.77635683940025E-14,3.96875));
#20486=CARTESIAN_POINT('Origin',(0.,0.,0.));
#20487=CARTESIAN_POINT('',(6.45286220549562E-15,140.,3.96875));
#20488=CARTESIAN_POINT('',(6.45286220549562E-15,140.,3.96875));
#20489=CARTESIAN_POINT('Origin',(6.93889390390723E-15,140.,0.));
#20490=CARTESIAN_POINT('Origin',(6.93889390390723E-15,140.,0.));
#20491=CARTESIAN_POINT('Origin',(0.,0.,0.));
#20492=CARTESIAN_POINT('',(0.,0.,0.));
#20493=CARTESIAN_POINT('Origin',(0.,49.,0.));
#20494=CARTESIAN_POINT('',(-3.98310247321554,49.,-4.94544180916756));
#20495=CARTESIAN_POINT('',(4.03547286927067,49.,-4.90280110971059));
#20496=CARTESIAN_POINT('Origin',(0.,49.,0.));
#20497=CARTESIAN_POINT('',(-4.5,50.,-5.81141118834299));
#20498=CARTESIAN_POINT('Ctrl Pts',(-4.49999999999977,49.9999999999993,-5.81141118834253));
#20499=CARTESIAN_POINT('Ctrl Pts',(-4.22074508491678,49.4597480146199,-5.34436370422895));
#20500=CARTESIAN_POINT('Ctrl Pts',(-3.98310247321565,48.9999999999999,-4.94544180916757));
#20501=CARTESIAN_POINT('',(4.50000000000003,50.,-5.8114111883431));
#20502=CARTESIAN_POINT('Origin',(0.,50.,0.));
#20503=CARTESIAN_POINT('Ctrl Pts',(4.03547286927078,49.,-4.90280110971056));
#20504=CARTESIAN_POINT('Ctrl Pts',(4.24803951147274,49.4575979057849,-5.32050921950116));
#20505=CARTESIAN_POINT('Ctrl Pts',(4.50000000000141,50.0000000000031,-5.81141118834603));
#20506=CARTESIAN_POINT('Origin',(0.,10.,0.));
#20507=CARTESIAN_POINT('',(-7.7765071745857E-16,10.,-6.35000000000001));
#20508=CARTESIAN_POINT('Origin',(0.,10.,0.));
#20509=CARTESIAN_POINT('',(-7.7765071745857E-16,18.,-6.35000000000001));
#20510=CARTESIAN_POINT('',(-7.7765071745857E-16,10.,-6.35000000000001));
#20511=CARTESIAN_POINT('',(-1.46216278437505,18.,-6.17936728087826));
#20512=CARTESIAN_POINT('Origin',(0.,18.,0.));
#20513=CARTESIAN_POINT('',(-1.46216278437505,44.122941089459,-6.17936728087826));
#20514=CARTESIAN_POINT('',(-1.46216278437505,10.,-6.17936728087826));
#20515=CARTESIAN_POINT('Origin',(-5.47117906535277E-12,41.2942125531358,
-1.69803060501295E-11));
#20516=CARTESIAN_POINT('',(1.71283721562501,44.,-6.11462907074245));
#20517=CARTESIAN_POINT('Origin',(-4.41341407864115E-12,40.3127294353338,
1.04150021940086E-11));
#20518=CARTESIAN_POINT('',(1.71283721562501,18.,-6.11462907074245));
#20519=CARTESIAN_POINT('',(1.71283721562501,10.,-6.11462907074245));
#20520=CARTESIAN_POINT('Origin',(0.,18.,0.));
#20521=CARTESIAN_POINT('Origin',(0.,50.,0.));
#20522=CARTESIAN_POINT('',(6.78069956542715,0.,-4.12625976562492));
#20523=CARTESIAN_POINT('',(-6.78069956542721,0.,-4.12625976562492));
#20524=CARTESIAN_POINT('Origin',(0.,0.,0.));
#20525=CARTESIAN_POINT('',(-6.96263988196173,-2.54796184151473E-11,3.81124023437512));
#20526=CARTESIAN_POINT('Ctrl Pts',(-6.78069956542709,-1.59594559789866E-15,
-4.12625976562516));
#20527=CARTESIAN_POINT('Ctrl Pts',(-6.78069956542709,0.20291602635612,-4.12625976562516));
#20528=CARTESIAN_POINT('Ctrl Pts',(-6.789971315478,0.40609151683513,-4.11113887165097));
#20529=CARTESIAN_POINT('Ctrl Pts',(-6.85001139901333,1.06933946691968,-4.01096526257536));
#20530=CARTESIAN_POINT('Ctrl Pts',(-6.93780786854016,1.50828047099799,-3.8638114398035));
#20531=CARTESIAN_POINT('Ctrl Pts',(-7.17422155741041,2.36061047309084,-3.40717387141783));
#20532=CARTESIAN_POINT('Ctrl Pts',(-7.32703301852759,2.75937873020496,-3.08105830459423));
#20533=CARTESIAN_POINT('Ctrl Pts',(-7.60736246330475,3.40131175443517,-2.3022040118231));
#20534=CARTESIAN_POINT('Ctrl Pts',(-7.73374530365473,3.64481097932461,-1.85477666749764));
#20535=CARTESIAN_POINT('Ctrl Pts',(-7.89829313943706,3.93499941473798,-0.912243104787409));
#20536=CARTESIAN_POINT('Ctrl Pts',(-7.93998719122528,3.99124892394717,-0.436363089125317));
#20537=CARTESIAN_POINT('Ctrl Pts',(-7.93483838332232,3.9308187778951,0.511588998034206));
#20538=CARTESIAN_POINT('Ctrl Pts',(-7.89016948894505,3.81908070047316,0.967194108666593));
#20539=CARTESIAN_POINT('Ctrl Pts',(-7.73156920749371,3.43283541545737,1.85744415264528));
#20540=CARTESIAN_POINT('Ctrl Pts',(-7.6131090943576,3.1475122718246,2.27716767192686));
#20541=CARTESIAN_POINT('Ctrl Pts',(-7.35583080822277,2.42434696900374,3.00933293642248));
#20542=CARTESIAN_POINT('Ctrl Pts',(-7.21682951488633,1.97770824086303,3.31262246589732));
#20543=CARTESIAN_POINT('Ctrl Pts',(-7.06811858761907,1.24745024754987,3.61345869274962));
#20544=CARTESIAN_POINT('Ctrl Pts',(-7.02926529552173,1.00441501289051,3.68734467939022));
#20545=CARTESIAN_POINT('Ctrl Pts',(-6.97647739981983,0.506199451376457,
3.7862620052672));
#20546=CARTESIAN_POINT('Ctrl Pts',(-6.96263988196164,0.254067613467043,
3.81124023437485));
#20547=CARTESIAN_POINT('Ctrl Pts',(-6.96263988196164,0.,3.81124023437485));
#20548=CARTESIAN_POINT('',(-9.72063396823213E-16,0.,7.93750000000001));
#20549=CARTESIAN_POINT('Origin',(0.,0.,0.));
#20550=CARTESIAN_POINT('',(-9.72063396823213E-16,50.,7.93750000000001));
#20551=CARTESIAN_POINT('',(-9.72063396823213E-16,50.,7.93750000000001));
#20552=CARTESIAN_POINT('',(-4.50000000000012,50.,-6.53864712689098));
#20553=CARTESIAN_POINT('Origin',(0.,50.,0.));
#20554=CARTESIAN_POINT('',(-1.46216278437508,44.122941089459,-7.80166560690648));
#20555=CARTESIAN_POINT('Origin',(-1.63441482570192E-11,41.2942125531507,
-2.83206791351631E-11));
#20556=CARTESIAN_POINT('',(-1.46216278437508,18.,-7.80166560690648));
#20557=CARTESIAN_POINT('',(-1.46216278437508,50.,-7.80166560690648));
#20558=CARTESIAN_POINT('',(1.71283721562494,18.,-7.75048997952832));
#20559=CARTESIAN_POINT('Origin',(0.,18.,0.));
#20560=CARTESIAN_POINT('',(1.71283721562494,44.,-7.75048997952832));
#20561=CARTESIAN_POINT('',(1.71283721562494,50.,-7.75048997952832));
#20562=CARTESIAN_POINT('',(4.49999999999992,50.,-6.53864712689095));
#20563=CARTESIAN_POINT('Origin',(-2.26108021195159E-11,40.3127294352942,
4.90707474654073E-11));
#20564=CARTESIAN_POINT('Origin',(0.,50.,0.));
#20565=CARTESIAN_POINT('',(6.96263988196147,0.,3.81124023437518));
#20566=CARTESIAN_POINT('Origin',(0.,0.,0.));
#20567=CARTESIAN_POINT('Ctrl Pts',(6.96263988196154,9.71445146547012E-16,
3.81124023437498));
#20568=CARTESIAN_POINT('Ctrl Pts',(6.96263988196154,0.445939065058851,3.81124023437498));
#20569=CARTESIAN_POINT('Ctrl Pts',(7.00600256018719,0.882552917010117,3.7345501133779));
#20570=CARTESIAN_POINT('Ctrl Pts',(7.16255453367982,1.7545618554345,3.42561203152615));
#20571=CARTESIAN_POINT('Ctrl Pts',(7.27981347983279,2.17438418007477,3.18093762861799));
#20572=CARTESIAN_POINT('Ctrl Pts',(7.53445421285187,2.94715506316683,2.52473565447381));
#20573=CARTESIAN_POINT('Ctrl Pts',(7.67173489201974,3.28625881372763,2.09625272246473));
#20574=CARTESIAN_POINT('Ctrl Pts',(7.8629249241042,3.75334095385897,1.17367468316625));
#20575=CARTESIAN_POINT('Ctrl Pts',(7.92235190096679,3.8959552204152,0.697053670144953));
#20576=CARTESIAN_POINT('Ctrl Pts',(7.94675012447075,3.99568166692586,-0.263277261294666));
#20577=CARTESIAN_POINT('Ctrl Pts',(7.91694647191713,3.96207512102207,-0.729006144604749));
#20578=CARTESIAN_POINT('Ctrl Pts',(7.78063473675749,3.73138702283732,-1.63778832271464));
#20579=CARTESIAN_POINT('Ctrl Pts',(7.67434248237991,3.53338352035958,-2.06587018517267));
#20580=CARTESIAN_POINT('Ctrl Pts',(7.41513175825483,2.9732220006111,-2.86618920547352));
#20581=CARTESIAN_POINT('Ctrl Pts',(7.26011037168438,2.59860363725,-3.22317703114952));
#20582=CARTESIAN_POINT('Ctrl Pts',(6.99433349067142,1.74884021981955,-3.76442418449406));
#20583=CARTESIAN_POINT('Ctrl Pts',(6.88384000315192,1.27946736789922,-3.95341867708105));
#20584=CARTESIAN_POINT('Ctrl Pts',(6.79611754991714,0.521986131736863,-4.10123268100205));
#20585=CARTESIAN_POINT('Ctrl Pts',(6.78069956542718,0.261208033678902,-4.12625976562502));
#20586=CARTESIAN_POINT('Ctrl Pts',(6.78069956542718,1.56125112837913E-16,
-4.12625976562502));
#20587=CARTESIAN_POINT('Origin',(0.,0.,0.));
#20588=CARTESIAN_POINT('Origin',(1.51267887105178E-12,0.,-150.));
#20589=CARTESIAN_POINT('Origin',(0.,0.,0.));
#20590=CARTESIAN_POINT('Origin',(1.51267887105178E-12,0.,-150.));
#20591=CARTESIAN_POINT('Origin',(0.,50.,0.));
#20592=CARTESIAN_POINT('',(4.49999999999989,50.,5.20417042793042E-14));
#20593=CARTESIAN_POINT('',(-4.50000000000012,50.,1.14491749414469E-13));
#20594=CARTESIAN_POINT('Origin',(1.71283721562496,18.,-40.0000000000001));
#20595=CARTESIAN_POINT('',(1.71283721562496,18.,-40.0000000000001));
#20596=CARTESIAN_POINT('',(1.71283721562496,44.,-40.0000000000001));
#20597=CARTESIAN_POINT('Origin',(-1.46216278437511,18.,-40.));
#20598=CARTESIAN_POINT('',(-1.46216278437511,18.,-40.));
#20599=CARTESIAN_POINT('Origin',(-1.46216278437511,44.122941089459,-40.));
#20600=CARTESIAN_POINT('',(-1.46216278437511,44.122941089459,-40.));
#20601=CARTESIAN_POINT('Origin',(-4.50000000000012,50.,-40.));
#20602=CARTESIAN_POINT('Origin',(1.71283721562496,44.,-40.0000000000001));
#20603=CARTESIAN_POINT('Origin',(1.51267887105178E-12,0.,-150.));
#20604=CARTESIAN_POINT('Origin',(0.,10.,0.));
#20605=CARTESIAN_POINT('',(0.,0.,0.));
#20606=CARTESIAN_POINT('',(0.,0.,0.));
#20607=CARTESIAN_POINT('',(41.1462220812905,-137.479353133212,-0.401944789973093));
#20608=CARTESIAN_POINT('',(41.751358612144,-125.232077853698,-0.361735996796731));
#20609=CARTESIAN_POINT('',(149.644183622419,-117.886188080489,-110.153154104068));
#20610=CARTESIAN_POINT('',(150.,-154.8299916788,0.));
#20611=CARTESIAN_POINT('',(150.,-114.063163481004,-1.16118052673198E-13));
#20612=CARTESIAN_POINT('',(150.,-87.483163481004,9.88592726529913E-16));
#20613=CARTESIAN_POINT('',(150.,-151.4099916788,0.));
#20614=CARTESIAN_POINT('',(150.,-451.4099916788,0.));
#20615=CARTESIAN_POINT('',(150.,-457.9349916788,5.55653613398821E-16));
#20616=CARTESIAN_POINT('',(152.56633504356,-84.063163481004,0.387673013115028));
#20617=CARTESIAN_POINT('',(150.401944789973,-137.479353133212,-108.853777918709));
#20618=CARTESIAN_POINT('',(258.85377791871,-137.479353133212,0.401944789973853));
#20619=CARTESIAN_POINT('',(149.598055210026,-137.479353133212,108.853777918709));
#20620=CARTESIAN_POINT('',(20.0961894323343,0.,-75.0000000000002));
#20621=CARTESIAN_POINT('',(75.0000000000003,0.,-129.903810567666));
#20622=CARTESIAN_POINT('',(150.000000000001,0.,-150.));
#20623=CARTESIAN_POINT('',(225.000000000001,0.,-129.903810567665));
#20624=CARTESIAN_POINT('',(279.903810567666,0.,-74.9999999999992));
#20625=CARTESIAN_POINT('',(300.,0.,1.04744440165294E-12));
#20626=CARTESIAN_POINT('',(279.903810567665,0.,75.0000000000011));
#20627=CARTESIAN_POINT('',(224.999999999999,0.,129.903810567666));
#20628=CARTESIAN_POINT('',(149.999999999998,0.,150.));
#20629=CARTESIAN_POINT('',(74.9999999999985,0.,129.903810567665));
#20630=CARTESIAN_POINT('',(20.0961894323332,0.,74.9999999999983));
#20631=UNCERTAINTY_MEASURE_WITH_UNIT(LENGTH_MEASURE(0.01),#20659,
'DISTANCE_ACCURACY_VALUE',
'Maximum model space distance between geometric entities at asserted c
onnectivities');
#20632=UNCERTAINTY_MEASURE_WITH_UNIT(LENGTH_MEASURE(0.01),#20659,
'DISTANCE_ACCURACY_VALUE',
'Maximum model space distance between geometric entities at asserted c
onnectivities');
#20633=UNCERTAINTY_MEASURE_WITH_UNIT(LENGTH_MEASURE(0.01),#20659,
'DISTANCE_ACCURACY_VALUE',
'Maximum model space distance between geometric entities at asserted c
onnectivities');
#20634=UNCERTAINTY_MEASURE_WITH_UNIT(LENGTH_MEASURE(0.01),#20659,
'DISTANCE_ACCURACY_VALUE',
'Maximum model space distance between geometric entities at asserted c
onnectivities');
#20635=UNCERTAINTY_MEASURE_WITH_UNIT(LENGTH_MEASURE(0.01),#20659,
'DISTANCE_ACCURACY_VALUE',
'Maximum model space distance between geometric entities at asserted c
onnectivities');
#20636=UNCERTAINTY_MEASURE_WITH_UNIT(LENGTH_MEASURE(0.01),#20659,
'DISTANCE_ACCURACY_VALUE',
'Maximum model space distance between geometric entities at asserted c
onnectivities');
#20637=UNCERTAINTY_MEASURE_WITH_UNIT(LENGTH_MEASURE(0.01),#20659,
'DISTANCE_ACCURACY_VALUE',
'Maximum model space distance between geometric entities at asserted c
onnectivities');
#20638=UNCERTAINTY_MEASURE_WITH_UNIT(LENGTH_MEASURE(0.01),#20659,
'DISTANCE_ACCURACY_VALUE',
'Maximum model space distance between geometric entities at asserted c
onnectivities');
#20639=UNCERTAINTY_MEASURE_WITH_UNIT(LENGTH_MEASURE(0.01),#20659,
'DISTANCE_ACCURACY_VALUE',
'Maximum model space distance between geometric entities at asserted c
onnectivities');
#20640=UNCERTAINTY_MEASURE_WITH_UNIT(LENGTH_MEASURE(0.01),#20659,
'DISTANCE_ACCURACY_VALUE',
'Maximum model space distance between geometric entities at asserted c
onnectivities');
#20641=UNCERTAINTY_MEASURE_WITH_UNIT(LENGTH_MEASURE(0.01),#20659,
'DISTANCE_ACCURACY_VALUE',
'Maximum model space distance between geometric entities at asserted c
onnectivities');
#20642=UNCERTAINTY_MEASURE_WITH_UNIT(LENGTH_MEASURE(0.01),#20659,
'DISTANCE_ACCURACY_VALUE',
'Maximum model space distance between geometric entities at asserted c
onnectivities');
#20643=UNCERTAINTY_MEASURE_WITH_UNIT(LENGTH_MEASURE(0.01),#20659,
'DISTANCE_ACCURACY_VALUE',
'Maximum model space distance between geometric entities at asserted c
onnectivities');
#20644=UNCERTAINTY_MEASURE_WITH_UNIT(LENGTH_MEASURE(0.01),#20659,
'DISTANCE_ACCURACY_VALUE',
'Maximum model space distance between geometric entities at asserted c
onnectivities');
#20645=(
GEOMETRIC_REPRESENTATION_CONTEXT(3)
GLOBAL_UNCERTAINTY_ASSIGNED_CONTEXT((#20631))
GLOBAL_UNIT_ASSIGNED_CONTEXT((#20659,#20661,#20662))
REPRESENTATION_CONTEXT('','3D')
);
#20646=(
GEOMETRIC_REPRESENTATION_CONTEXT(3)
GLOBAL_UNCERTAINTY_ASSIGNED_CONTEXT((#20632))
GLOBAL_UNIT_ASSIGNED_CONTEXT((#20659,#20661,#20662))
REPRESENTATION_CONTEXT('','3D')
);
#20647=(
GEOMETRIC_REPRESENTATION_CONTEXT(3)
GLOBAL_UNCERTAINTY_ASSIGNED_CONTEXT((#20633))
GLOBAL_UNIT_ASSIGNED_CONTEXT((#20659,#20661,#20662))
REPRESENTATION_CONTEXT('','3D')
);
#20648=(
GEOMETRIC_REPRESENTATION_CONTEXT(3)
GLOBAL_UNCERTAINTY_ASSIGNED_CONTEXT((#20634))
GLOBAL_UNIT_ASSIGNED_CONTEXT((#20659,#20661,#20662))
REPRESENTATION_CONTEXT('','3D')
);
#20649=(
GEOMETRIC_REPRESENTATION_CONTEXT(3)
GLOBAL_UNCERTAINTY_ASSIGNED_CONTEXT((#20635))
GLOBAL_UNIT_ASSIGNED_CONTEXT((#20659,#20661,#20662))
REPRESENTATION_CONTEXT('','3D')
);
#20650=(
GEOMETRIC_REPRESENTATION_CONTEXT(3)
GLOBAL_UNCERTAINTY_ASSIGNED_CONTEXT((#20636))
GLOBAL_UNIT_ASSIGNED_CONTEXT((#20659,#20661,#20662))
REPRESENTATION_CONTEXT('','3D')
);
#20651=(
GEOMETRIC_REPRESENTATION_CONTEXT(3)
GLOBAL_UNCERTAINTY_ASSIGNED_CONTEXT((#20637))
GLOBAL_UNIT_ASSIGNED_CONTEXT((#20659,#20661,#20662))
REPRESENTATION_CONTEXT('','3D')
);
#20652=(
GEOMETRIC_REPRESENTATION_CONTEXT(3)
GLOBAL_UNCERTAINTY_ASSIGNED_CONTEXT((#20638))
GLOBAL_UNIT_ASSIGNED_CONTEXT((#20659,#20661,#20662))
REPRESENTATION_CONTEXT('','3D')
);
#20653=(
GEOMETRIC_REPRESENTATION_CONTEXT(3)
GLOBAL_UNCERTAINTY_ASSIGNED_CONTEXT((#20639))
GLOBAL_UNIT_ASSIGNED_CONTEXT((#20659,#20661,#20662))
REPRESENTATION_CONTEXT('','3D')
);
#20654=(
GEOMETRIC_REPRESENTATION_CONTEXT(3)
GLOBAL_UNCERTAINTY_ASSIGNED_CONTEXT((#20640))
GLOBAL_UNIT_ASSIGNED_CONTEXT((#20659,#20661,#20662))
REPRESENTATION_CONTEXT('','3D')
);
#20655=(
GEOMETRIC_REPRESENTATION_CONTEXT(3)
GLOBAL_UNCERTAINTY_ASSIGNED_CONTEXT((#20641))
GLOBAL_UNIT_ASSIGNED_CONTEXT((#20659,#20661,#20662))
REPRESENTATION_CONTEXT('','3D')
);
#20656=(
GEOMETRIC_REPRESENTATION_CONTEXT(3)
GLOBAL_UNCERTAINTY_ASSIGNED_CONTEXT((#20642))
GLOBAL_UNIT_ASSIGNED_CONTEXT((#20659,#20661,#20662))
REPRESENTATION_CONTEXT('','3D')
);
#20657=(
GEOMETRIC_REPRESENTATION_CONTEXT(3)
GLOBAL_UNCERTAINTY_ASSIGNED_CONTEXT((#20643))
GLOBAL_UNIT_ASSIGNED_CONTEXT((#20659,#20661,#20662))
REPRESENTATION_CONTEXT('','3D')
);
#20658=(
GEOMETRIC_REPRESENTATION_CONTEXT(3)
GLOBAL_UNCERTAINTY_ASSIGNED_CONTEXT((#20644))
GLOBAL_UNIT_ASSIGNED_CONTEXT((#20659,#20661,#20662))
REPRESENTATION_CONTEXT('','3D')
);
#20659=(
LENGTH_UNIT()
NAMED_UNIT(*)
SI_UNIT(.MILLI.,.METRE.)
);
#20660=(
LENGTH_UNIT()
NAMED_UNIT(*)
SI_UNIT($,.METRE.)
);
#20661=(
NAMED_UNIT(*)
PLANE_ANGLE_UNIT()
SI_UNIT($,.RADIAN.)
);
#20662=(
NAMED_UNIT(*)
SI_UNIT($,.STERADIAN.)
SOLID_ANGLE_UNIT()
);
#20663=SHAPE_DEFINITION_REPRESENTATION(#20676,#20715);
#20664=SHAPE_DEFINITION_REPRESENTATION(#20677,#20716);
#20665=SHAPE_DEFINITION_REPRESENTATION(#20678,#20717);
#20666=SHAPE_DEFINITION_REPRESENTATION(#20679,#20718);
#20667=SHAPE_DEFINITION_REPRESENTATION(#20680,#20719);
#20668=SHAPE_DEFINITION_REPRESENTATION(#20681,#20720);
#20669=SHAPE_DEFINITION_REPRESENTATION(#20682,#20721);
#20670=SHAPE_DEFINITION_REPRESENTATION(#20683,#20722);
#20671=SHAPE_DEFINITION_REPRESENTATION(#20684,#20723);
#20672=SHAPE_DEFINITION_REPRESENTATION(#20685,#20724);
#20673=SHAPE_DEFINITION_REPRESENTATION(#20686,#20725);
#20674=SHAPE_DEFINITION_REPRESENTATION(#20687,#20726);
#20675=SHAPE_DEFINITION_REPRESENTATION(#20688,#20727);
#20676=PRODUCT_DEFINITION_SHAPE('',$,#20729);
#20677=PRODUCT_DEFINITION_SHAPE('',$,#20730);
#20678=PRODUCT_DEFINITION_SHAPE('',$,#20731);
#20679=PRODUCT_DEFINITION_SHAPE('',$,#20732);
#20680=PRODUCT_DEFINITION_SHAPE('',$,#20733);
#20681=PRODUCT_DEFINITION_SHAPE('',$,#20734);
#20682=PRODUCT_DEFINITION_SHAPE('',$,#20735);
#20683=PRODUCT_DEFINITION_SHAPE('',$,#20736);
#20684=PRODUCT_DEFINITION_SHAPE('',$,#20737);
#20685=PRODUCT_DEFINITION_SHAPE('',$,#20738);
#20686=PRODUCT_DEFINITION_SHAPE('',$,#20739);
#20687=PRODUCT_DEFINITION_SHAPE('',$,#20740);
#20688=PRODUCT_DEFINITION_SHAPE('',$,#20741);
#20689=PRODUCT_DEFINITION_SHAPE($,$,#89);
#20690=PRODUCT_DEFINITION_SHAPE($,$,#90);
#20691=PRODUCT_DEFINITION_SHAPE($,$,#91);
#20692=PRODUCT_DEFINITION_SHAPE($,$,#92);
#20693=PRODUCT_DEFINITION_SHAPE($,$,#93);
#20694=PRODUCT_DEFINITION_SHAPE($,$,#94);
#20695=PRODUCT_DEFINITION_SHAPE($,$,#95);
#20696=PRODUCT_DEFINITION_SHAPE($,$,#96);
#20697=PRODUCT_DEFINITION_SHAPE($,$,#97);
#20698=PRODUCT_DEFINITION_SHAPE($,$,#98);
#20699=PRODUCT_DEFINITION_SHAPE($,$,#99);
#20700=PRODUCT_DEFINITION_SHAPE($,$,#100);
#20701=PRODUCT_DEFINITION_SHAPE($,$,#101);
#20702=PRODUCT_DEFINITION_SHAPE($,$,#102);
#20703=PRODUCT_DEFINITION_SHAPE($,$,#103);
#20704=PRODUCT_DEFINITION_SHAPE($,$,#104);
#20705=PRODUCT_DEFINITION_SHAPE($,$,#105);
#20706=PRODUCT_DEFINITION_SHAPE($,$,#106);
#20707=PRODUCT_DEFINITION_SHAPE($,$,#107);
#20708=PRODUCT_DEFINITION_SHAPE($,$,#108);
#20709=PRODUCT_DEFINITION_SHAPE($,$,#109);
#20710=PRODUCT_DEFINITION_SHAPE($,$,#110);
#20711=PRODUCT_DEFINITION_SHAPE($,$,#111);
#20712=PRODUCT_DEFINITION_SHAPE($,$,#112);
#20713=PRODUCT_DEFINITION_SHAPE($,$,#113);
#20714=PRODUCT_DEFINITION_SHAPE($,$,#114);
#20715=SHAPE_REPRESENTATION('',(#3796,#4103,#4104,#4105,#4106,#4107,#4108,
#4109,#4110,#4111,#4112,#4113,#4114,#4115,#4116,#4117,#4118,#4119,#4120,
#4121,#4122,#4123,#4124,#4125,#4126,#4127,#4128),#20645);
#20716=SHAPE_REPRESENTATION('',(#3797),#20646);
#20717=SHAPE_REPRESENTATION('',(#3801),#20647);
#20718=SHAPE_REPRESENTATION('',(#3807),#20648);
#20719=SHAPE_REPRESENTATION('',(#3813),#20649);
#20720=SHAPE_REPRESENTATION('',(#3932),#20650);
#20721=SHAPE_REPRESENTATION('',(#3966),#20651);
#20722=SHAPE_REPRESENTATION('',(#3972),#20652);
#20723=SHAPE_REPRESENTATION('',(#3981),#20653);
#20724=SHAPE_REPRESENTATION('',(#3990),#20654);
#20725=SHAPE_REPRESENTATION('',(#4015),#20655);
#20726=SHAPE_REPRESENTATION('',(#4066),#20656);
#20727=SHAPE_REPRESENTATION('',(#4072),#20657);
#20728=PRODUCT_DEFINITION_CONTEXT('part definition',#20769,'design');
#20729=PRODUCT_DEFINITION('MAT-020','MAT-020',#20742,#20728);
#20730=PRODUCT_DEFINITION('Ring','Ring',#20743,#20728);
#20731=PRODUCT_DEFINITION('Brace Rod','Brace Rod',#20744,#20728);
#20732=PRODUCT_DEFINITION('Brace Rod 2','Brace Rod 2',#20745,#20728);
#20733=PRODUCT_DEFINITION('Rotating Hub','Rotating Hub',#20746,#20728);
#20734=PRODUCT_DEFINITION('cover','Cover',#20747,#20728);
#20735=PRODUCT_DEFINITION('Cover Plate','Cover Plate',#20748,#20728);
#20736=PRODUCT_DEFINITION('Bottom Cover','Bottom Cover',#20749,#20728);
#20737=PRODUCT_DEFINITION('Tube','Tube',#20750,#20728);
#20738=PRODUCT_DEFINITION('Base plate','Base Plate',#20751,#20728);
#20739=PRODUCT_DEFINITION('Rotating Square Bar','Rotating Square Bar',#20752,
#20728);
#20740=PRODUCT_DEFINITION('Post','Post',#20753,#20728);
#20741=PRODUCT_DEFINITION('Pivot pin','Pivot Pin',#20754,#20728);
#20742=PRODUCT_DEFINITION_FORMATION('',$,#20771);
#20743=PRODUCT_DEFINITION_FORMATION('',$,#20772);
#20744=PRODUCT_DEFINITION_FORMATION('',$,#20773);
#20745=PRODUCT_DEFINITION_FORMATION('',$,#20774);
#20746=PRODUCT_DEFINITION_FORMATION('',$,#20775);
#20747=PRODUCT_DEFINITION_FORMATION('',$,#20776);
#20748=PRODUCT_DEFINITION_FORMATION('',$,#20777);
#20749=PRODUCT_DEFINITION_FORMATION('',$,#20778);
#20750=PRODUCT_DEFINITION_FORMATION('',$,#20779);
#20751=PRODUCT_DEFINITION_FORMATION('',$,#20780);
#20752=PRODUCT_DEFINITION_FORMATION('',$,#20781);
#20753=PRODUCT_DEFINITION_FORMATION('',$,#20782);
#20754=PRODUCT_DEFINITION_FORMATION('',$,#20783);
#20755=PRODUCT_RELATED_PRODUCT_CATEGORY('MAT-020','MAT-020',(#20771));
#20756=PRODUCT_RELATED_PRODUCT_CATEGORY('Ring','Ring',(#20772));
#20757=PRODUCT_RELATED_PRODUCT_CATEGORY('Brace Rod','Brace Rod',(#20773));
#20758=PRODUCT_RELATED_PRODUCT_CATEGORY('Brace Rod 2','Brace Rod 2',(#20774));
#20759=PRODUCT_RELATED_PRODUCT_CATEGORY('Rotating Hub','Rotating Hub',(#20775));
#20760=PRODUCT_RELATED_PRODUCT_CATEGORY('Cover','Cover',(#20776));
#20761=PRODUCT_RELATED_PRODUCT_CATEGORY('Cover Plate','Cover Plate',(#20777));
#20762=PRODUCT_RELATED_PRODUCT_CATEGORY('Bottom Cover','Bottom Cover',(#20778));
#20763=PRODUCT_RELATED_PRODUCT_CATEGORY('Tube','Tube',(#20779));
#20764=PRODUCT_RELATED_PRODUCT_CATEGORY('Base Plate','Base Plate',(#20780));
#20765=PRODUCT_RELATED_PRODUCT_CATEGORY('Rotating Square Bar',
'Rotating Square Bar',(#20781));
#20766=PRODUCT_RELATED_PRODUCT_CATEGORY('Post','Post',(#20782));
#20767=PRODUCT_RELATED_PRODUCT_CATEGORY('Pivot Pin','Pivot Pin',(#20783));
#20768=APPLICATION_PROTOCOL_DEFINITION('international standard',
'automotive_design',2009,#20769);
#20769=APPLICATION_CONTEXT(
'Core Data for Automotive Mechanical Design Process');
#20770=PRODUCT_CONTEXT('part definition',#20769,'mechanical');
#20771=PRODUCT('MAT-020','MAT-020','STEP AP214',(#20770));
#20772=PRODUCT('Ring','Ring',$,(#20770));
#20773=PRODUCT('Brace Rod','Brace Rod',$,(#20770));
#20774=PRODUCT('Brace Rod 2','Brace Rod 2',$,(#20770));
#20775=PRODUCT('Rotating Hub','Rotating Hub',$,(#20770));
#20776=PRODUCT('cover','Cover',$,(#20770));
#20777=PRODUCT('Cover Plate','Cover Plate',$,(#20770));
#20778=PRODUCT('Bottom Cover','Bottom Cover',$,(#20770));
#20779=PRODUCT('Tube','Tube',$,(#20770));
#20780=PRODUCT('Base plate','Base Plate','Base plate',(#20770));
#20781=PRODUCT('Rotating Square Bar','Rotating Square Bar',$,(#20770));
#20782=PRODUCT('Post','Post',$,(#20770));
#20783=PRODUCT('Pivot pin','Pivot Pin','Pivot pin',(#20770));
#20784=PRESENTATION_STYLE_ASSIGNMENT((#20789));
#20785=PRESENTATION_STYLE_ASSIGNMENT((#20790));
#20786=PRESENTATION_STYLE_ASSIGNMENT((#20791));
#20787=PRESENTATION_STYLE_ASSIGNMENT((#20792));
#20788=PRESENTATION_STYLE_ASSIGNMENT((#20793));
#20789=SURFACE_STYLE_USAGE(.BOTH.,#20794);
#20790=SURFACE_STYLE_USAGE(.BOTH.,#20795);
#20791=SURFACE_STYLE_USAGE(.BOTH.,#20796);
#20792=SURFACE_STYLE_USAGE(.BOTH.,#20797);
#20793=SURFACE_STYLE_USAGE(.BOTH.,#20798);
#20794=SURFACE_SIDE_STYLE('',(#20799));
#20795=SURFACE_SIDE_STYLE('',(#20800));
#20796=SURFACE_SIDE_STYLE('',(#20801));
#20797=SURFACE_SIDE_STYLE('',(#20802));
#20798=SURFACE_SIDE_STYLE('',(#20803));
#20799=SURFACE_STYLE_FILL_AREA(#20804);
#20800=SURFACE_STYLE_FILL_AREA(#20805);
#20801=SURFACE_STYLE_FILL_AREA(#20806);
#20802=SURFACE_STYLE_FILL_AREA(#20807);
#20803=SURFACE_STYLE_FILL_AREA(#20808);
#20804=FILL_AREA_STYLE('Steel - Satin',(#20809));
#20805=FILL_AREA_STYLE('Opaque(97,158,199)',(#20810));
#20806=FILL_AREA_STYLE('Opaque(61,176,222)',(#20811));
#20807=FILL_AREA_STYLE('Opaque(227,224,212)',(#20812));
#20808=FILL_AREA_STYLE('Opaque(20,51,87)',(#20813));
#20809=FILL_AREA_STYLE_COLOUR('Steel - Satin',#20814);
#20810=FILL_AREA_STYLE_COLOUR('Opaque(97,158,199)',#20815);
#20811=FILL_AREA_STYLE_COLOUR('Opaque(61,176,222)',#20816);
#20812=FILL_AREA_STYLE_COLOUR('Opaque(227,224,212)',#20817);
#20813=FILL_AREA_STYLE_COLOUR('Opaque(20,51,87)',#20818);
#20814=COLOUR_RGB('Steel - Satin',0.627450980392157,0.627450980392157,0.627450980392157);
#20815=COLOUR_RGB('Opaque(97,158,199)',0.380392156862745,0.619607843137255,
0.780392156862745);
#20816=COLOUR_RGB('Opaque(61,176,222)',0.23921568627451,0.690196078431373,
0.870588235294118);
#20817=COLOUR_RGB('Opaque(227,224,212)',0.890196078431372,0.87843137254902,
0.831372549019608);
#20818=COLOUR_RGB('Opaque(20,51,87)',0.0784313725490196,0.2,0.341176470588235);
ENDSEC;
END-ISO-10303-21;
